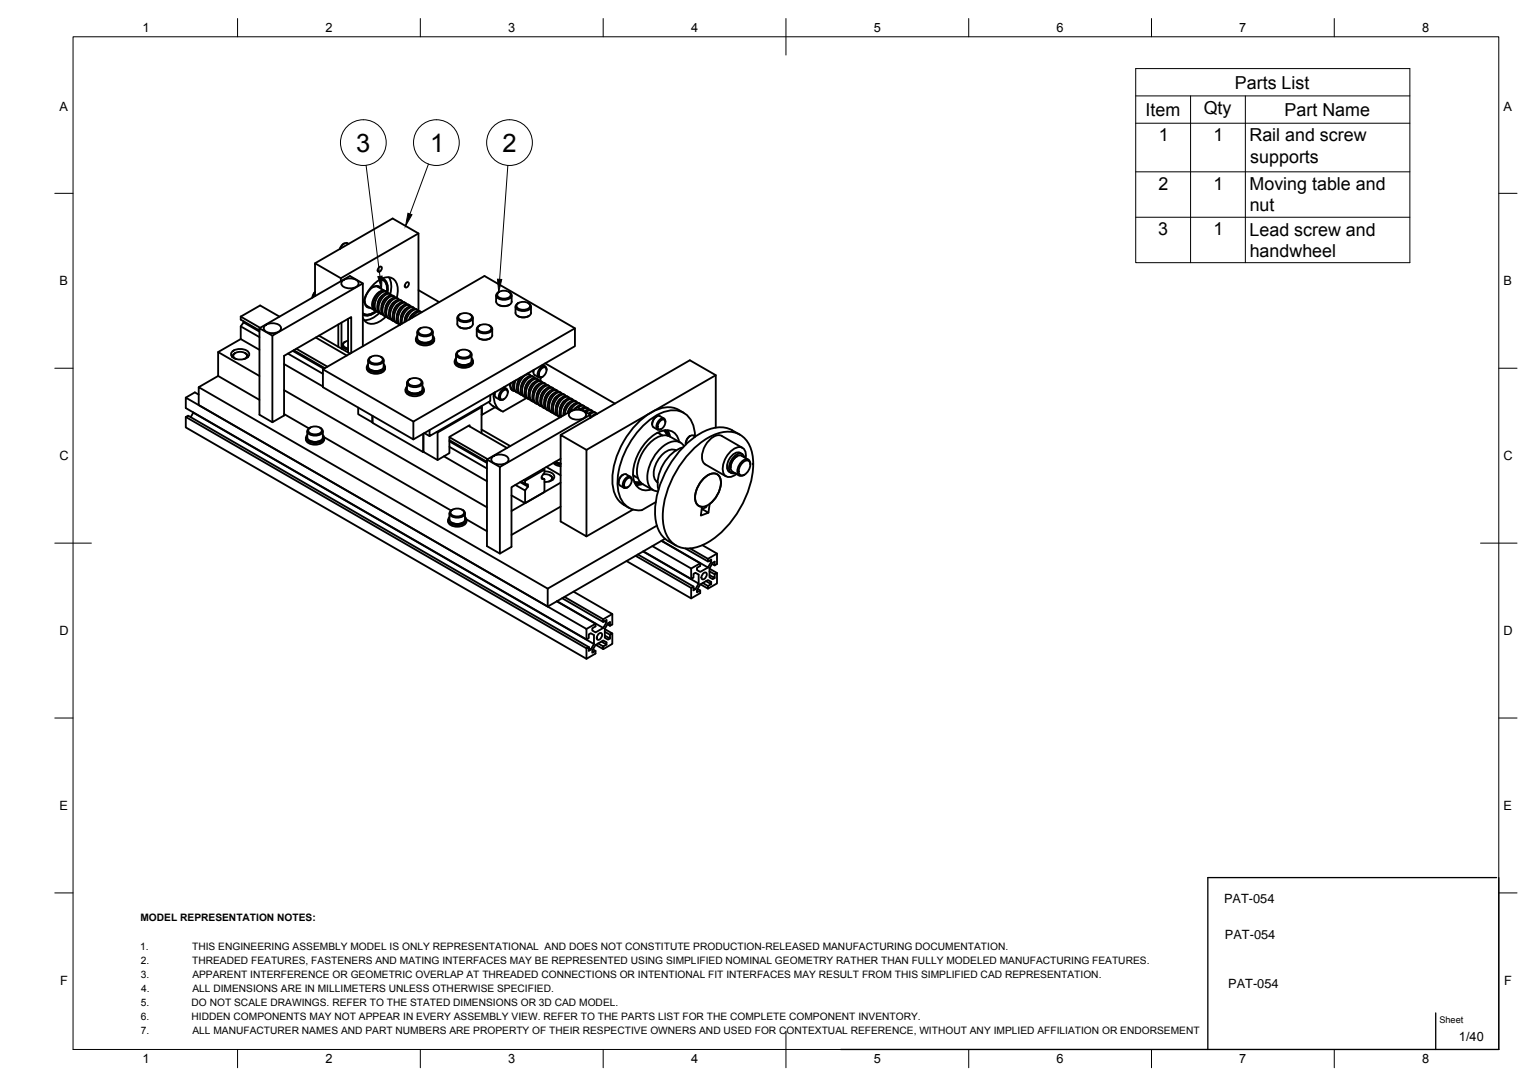
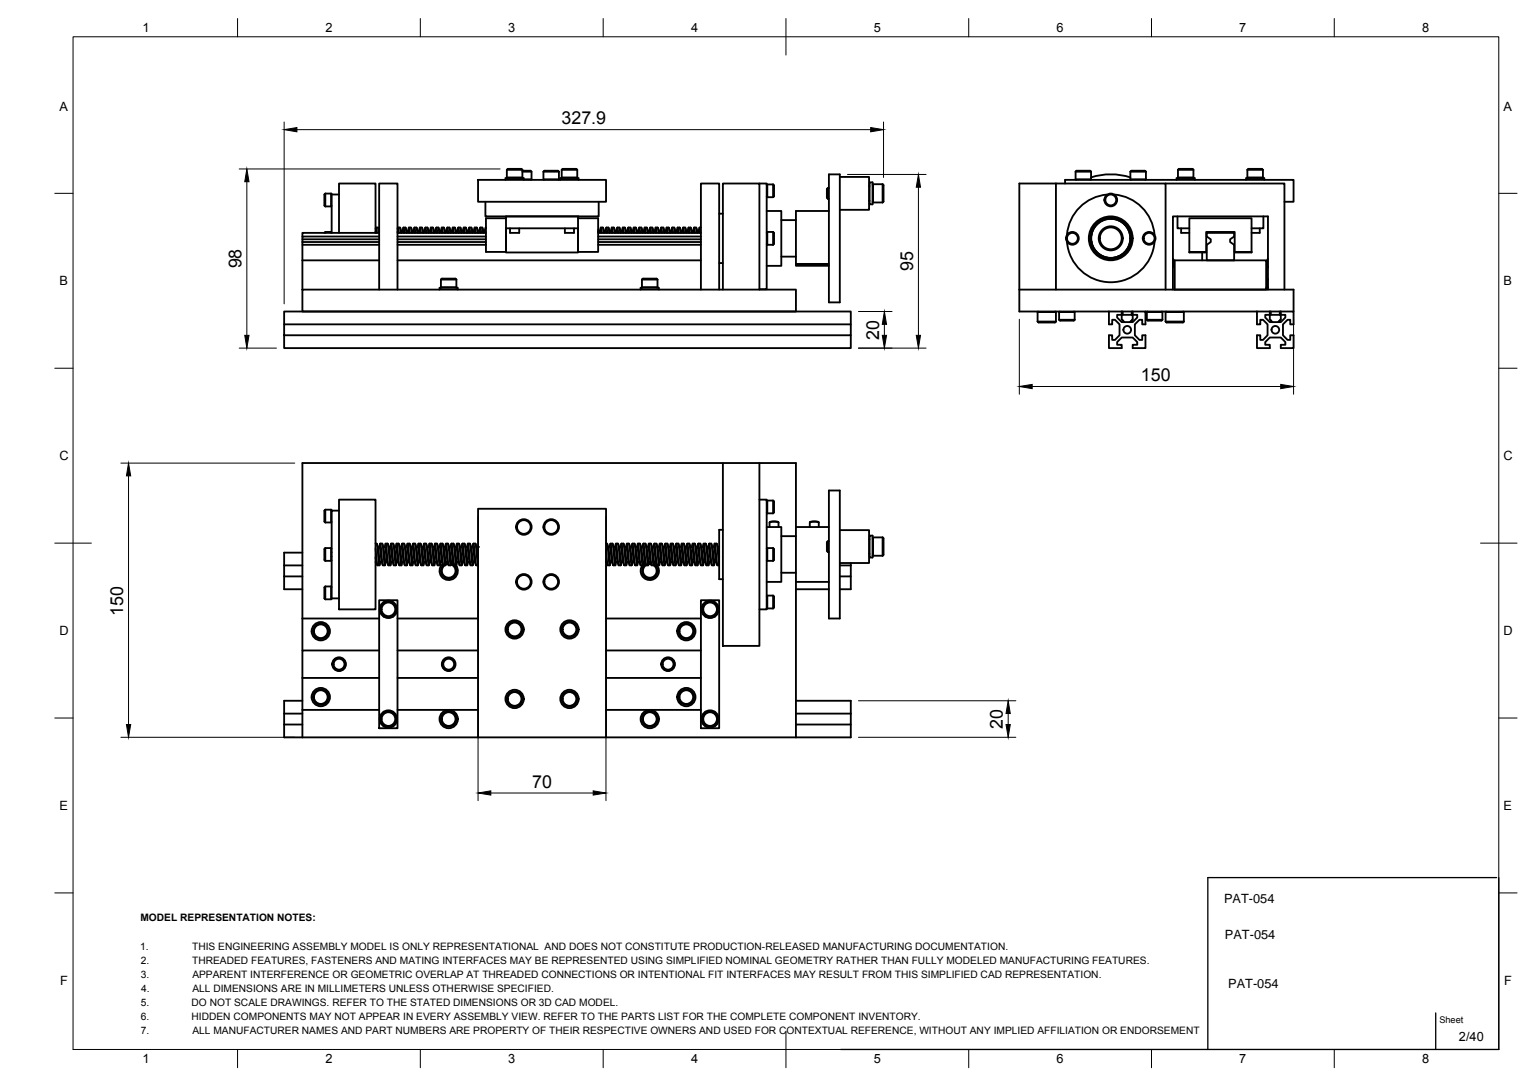
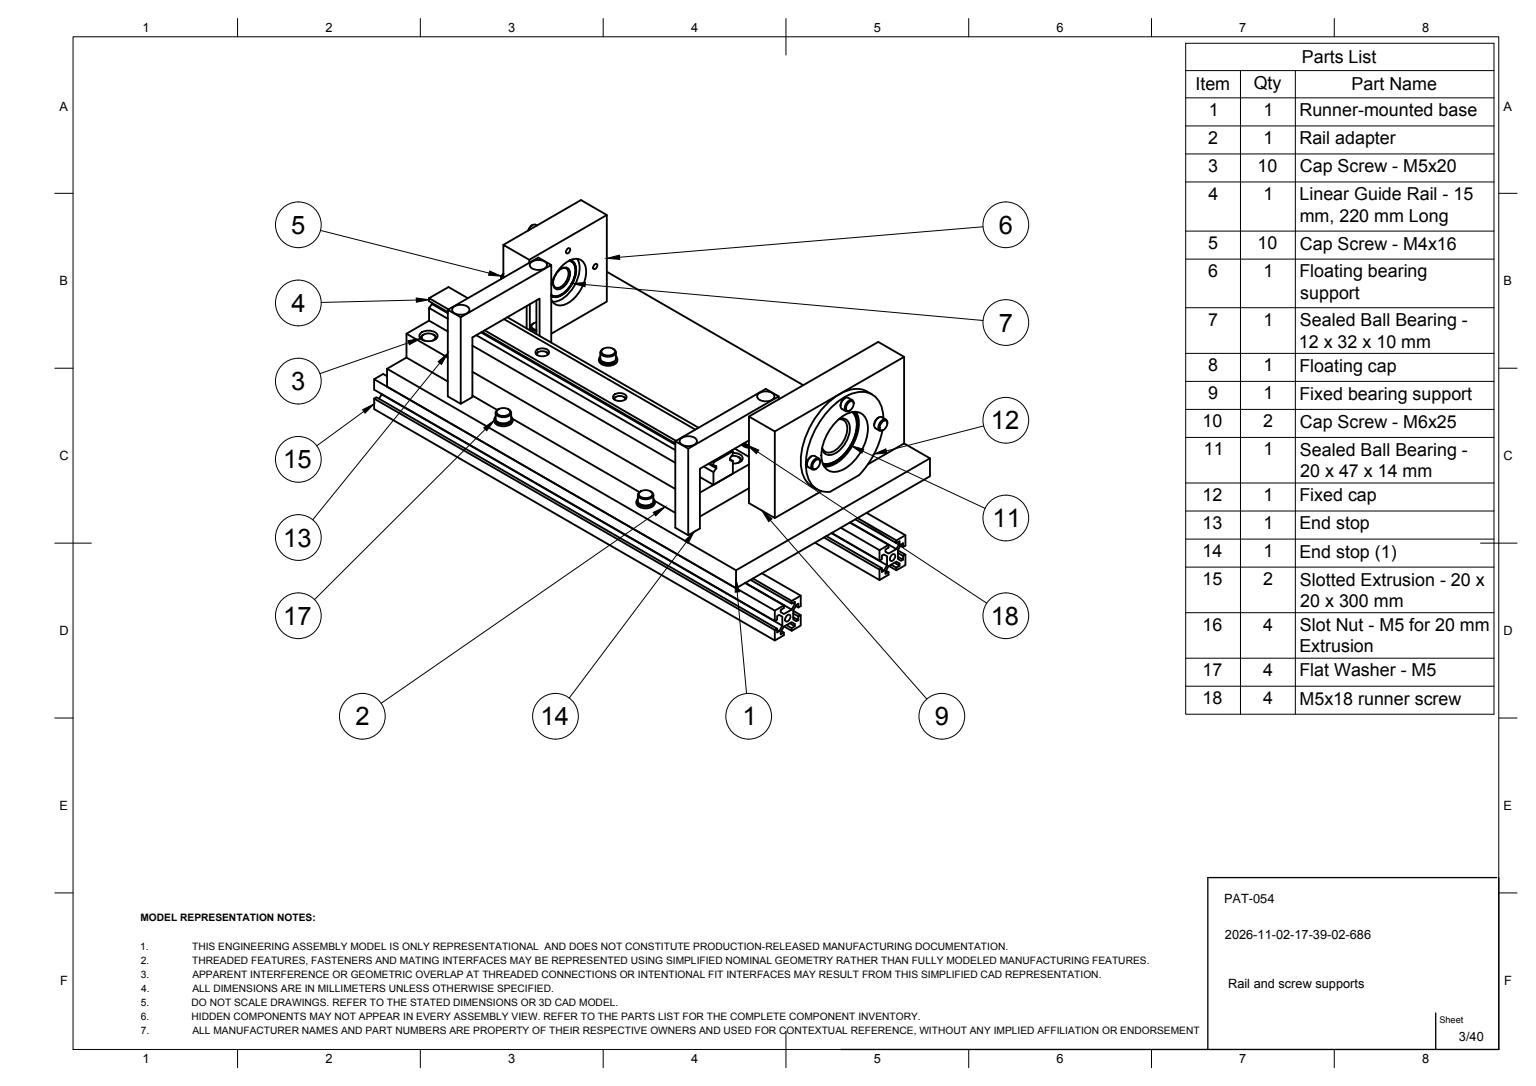
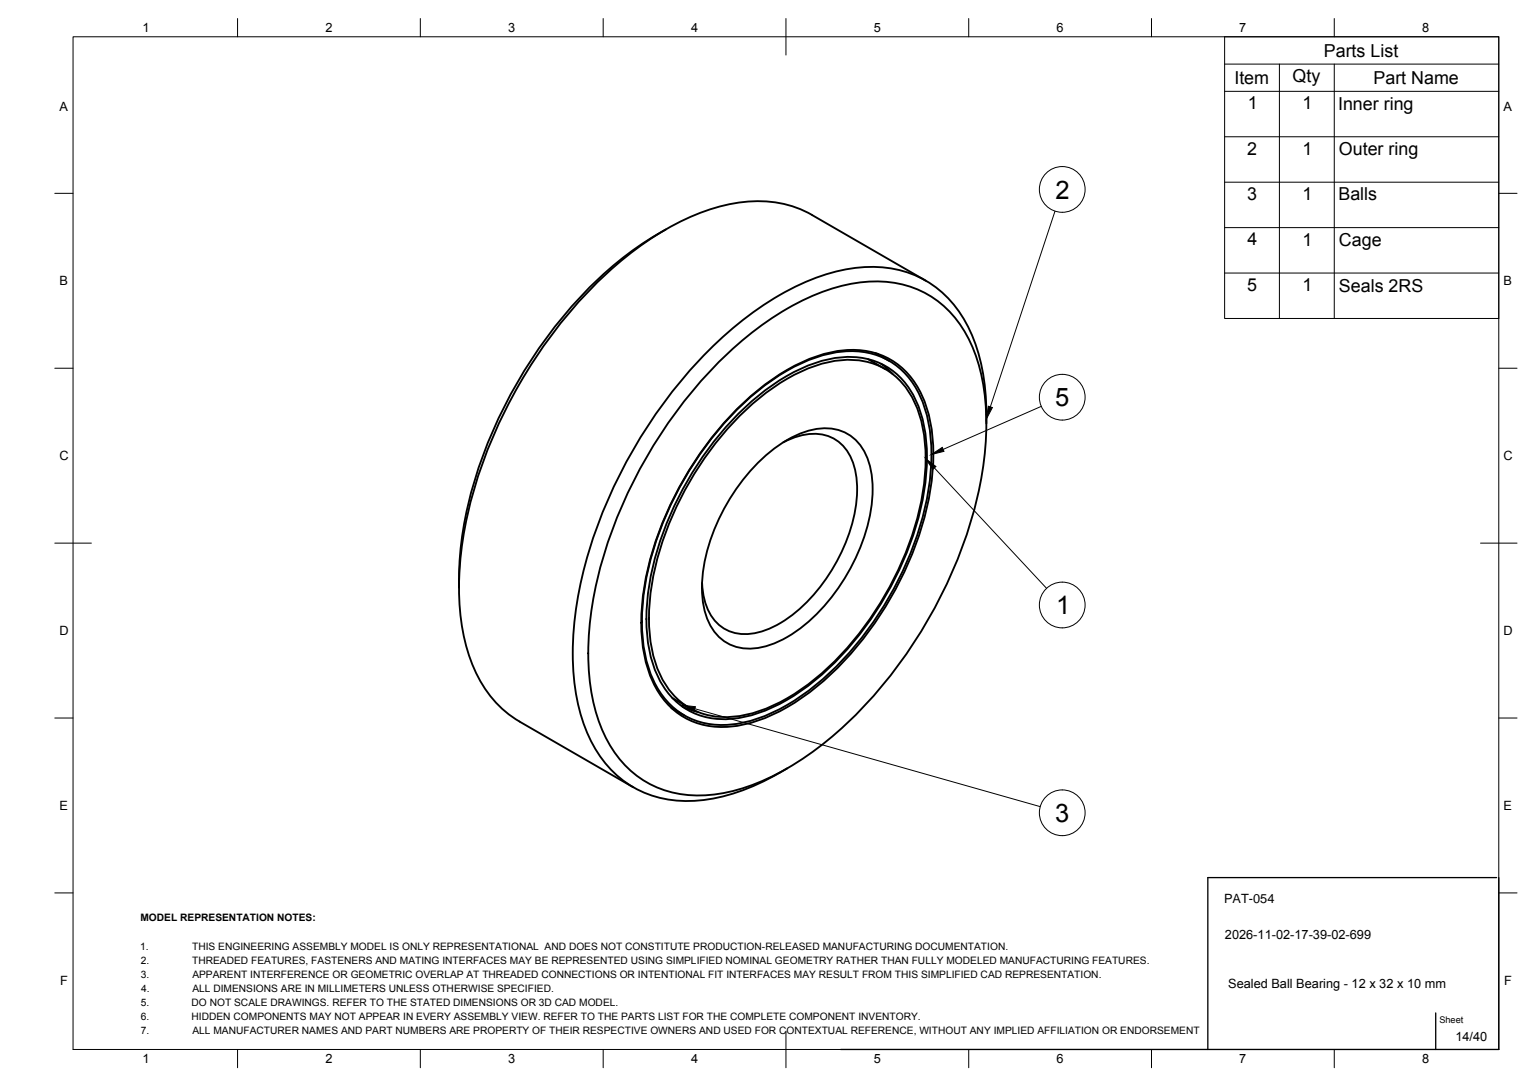
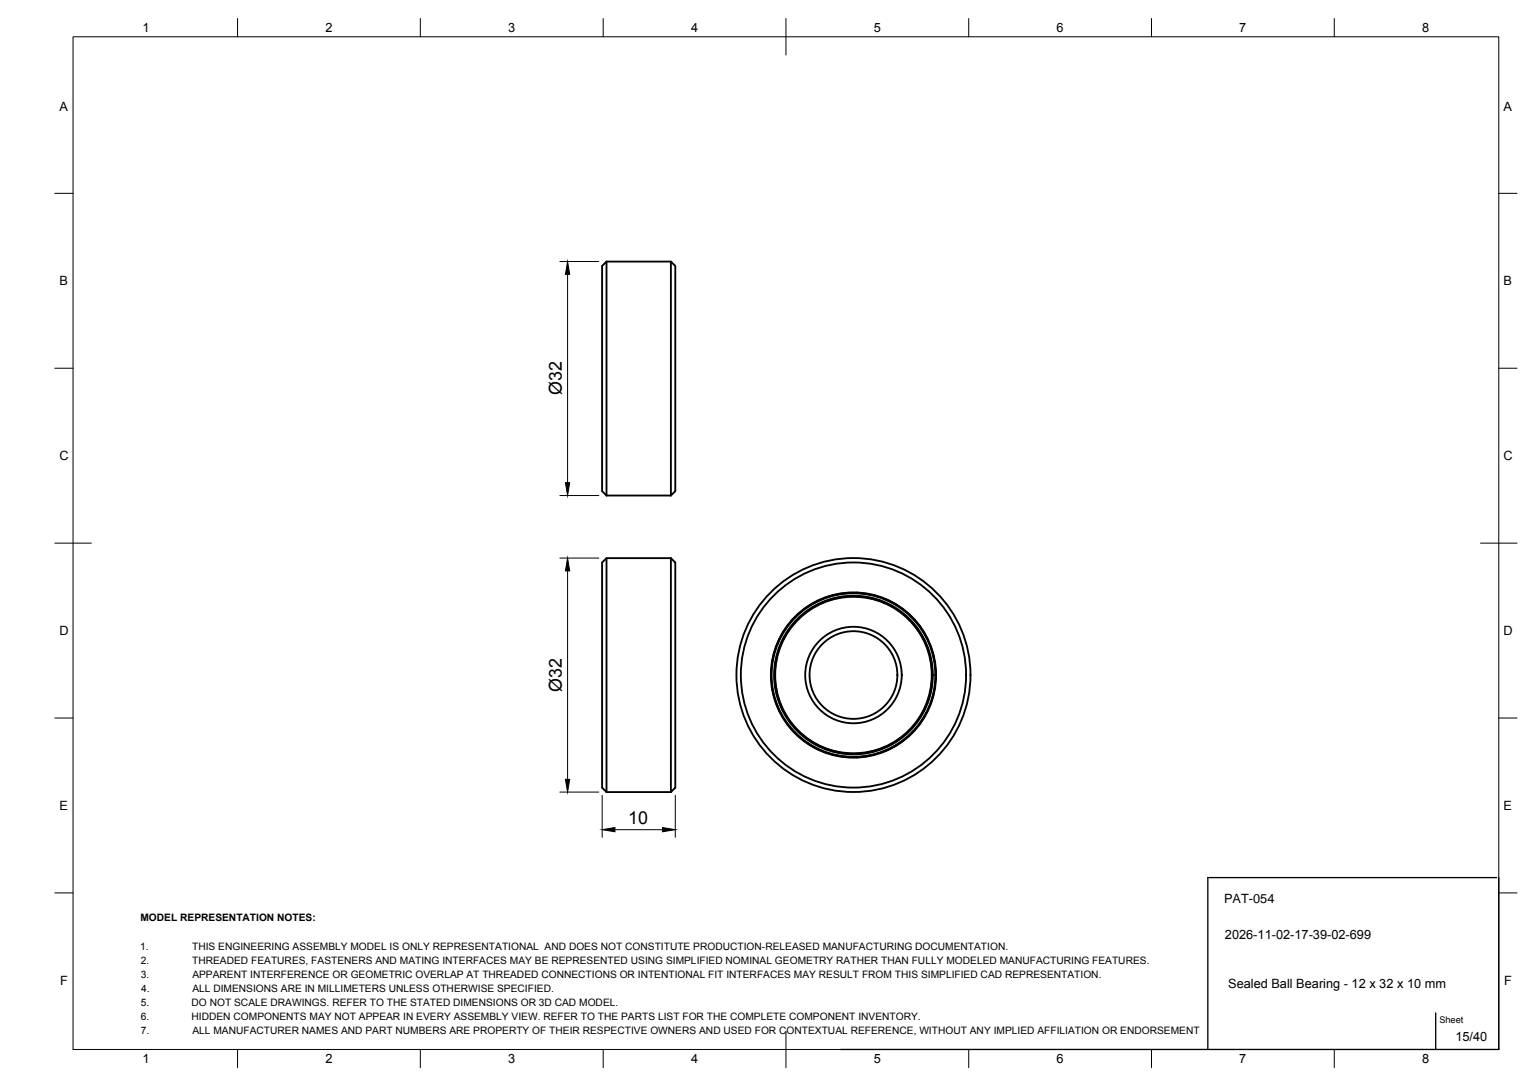
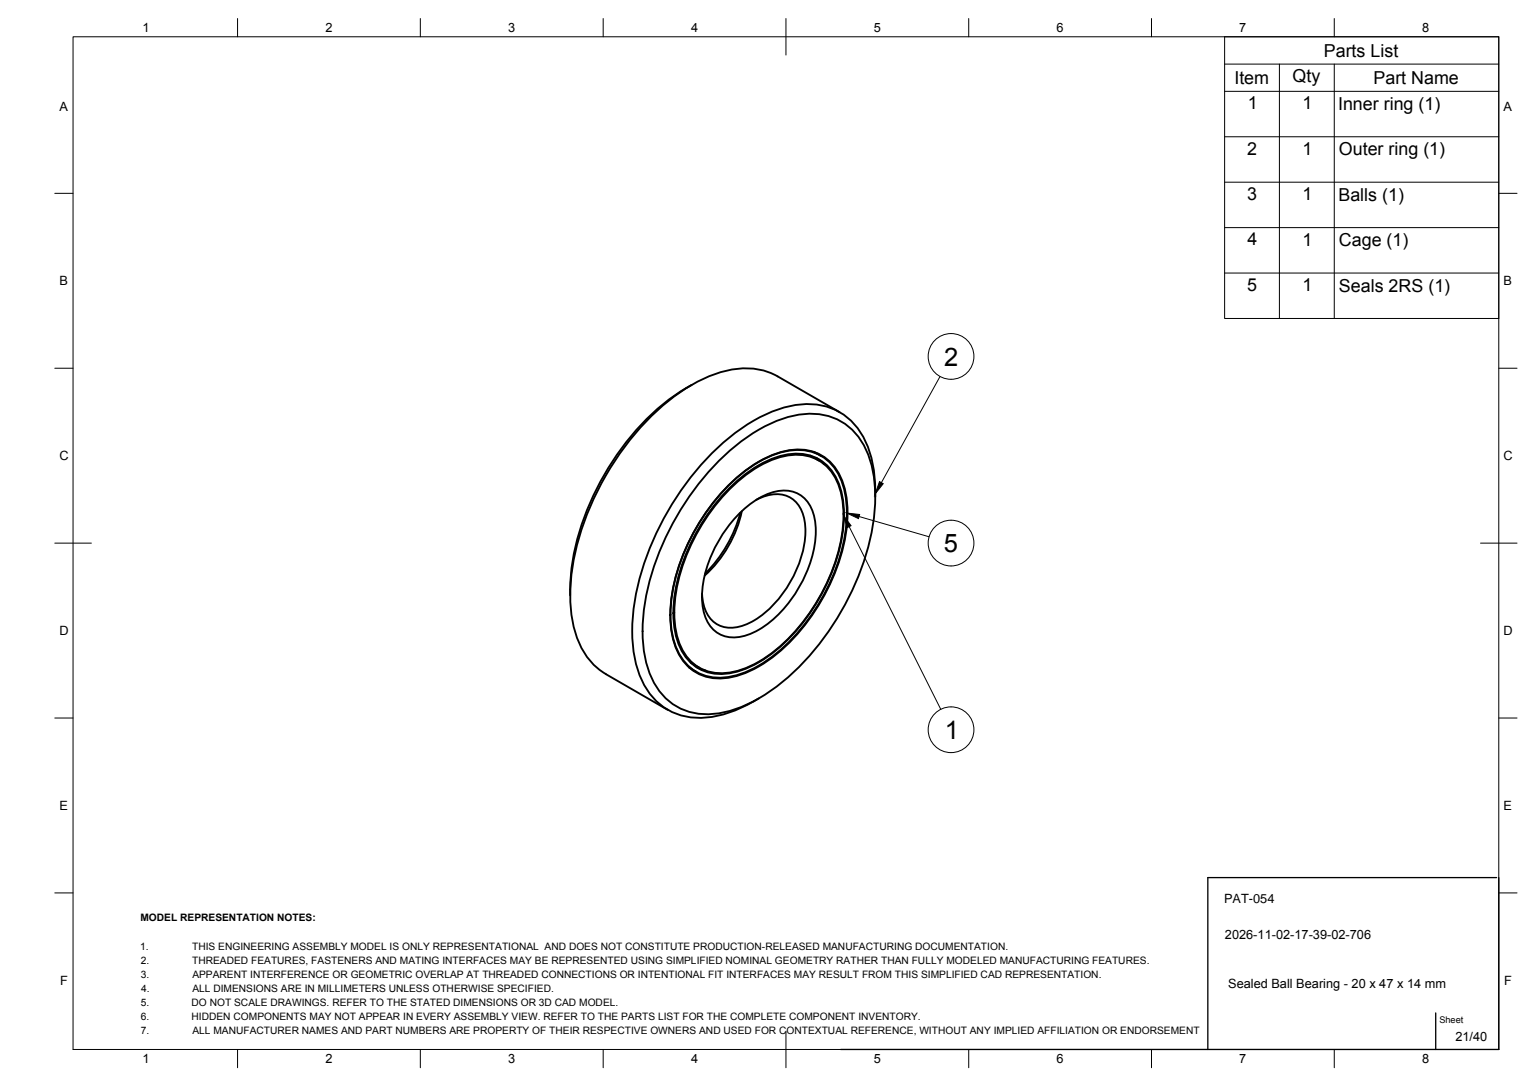
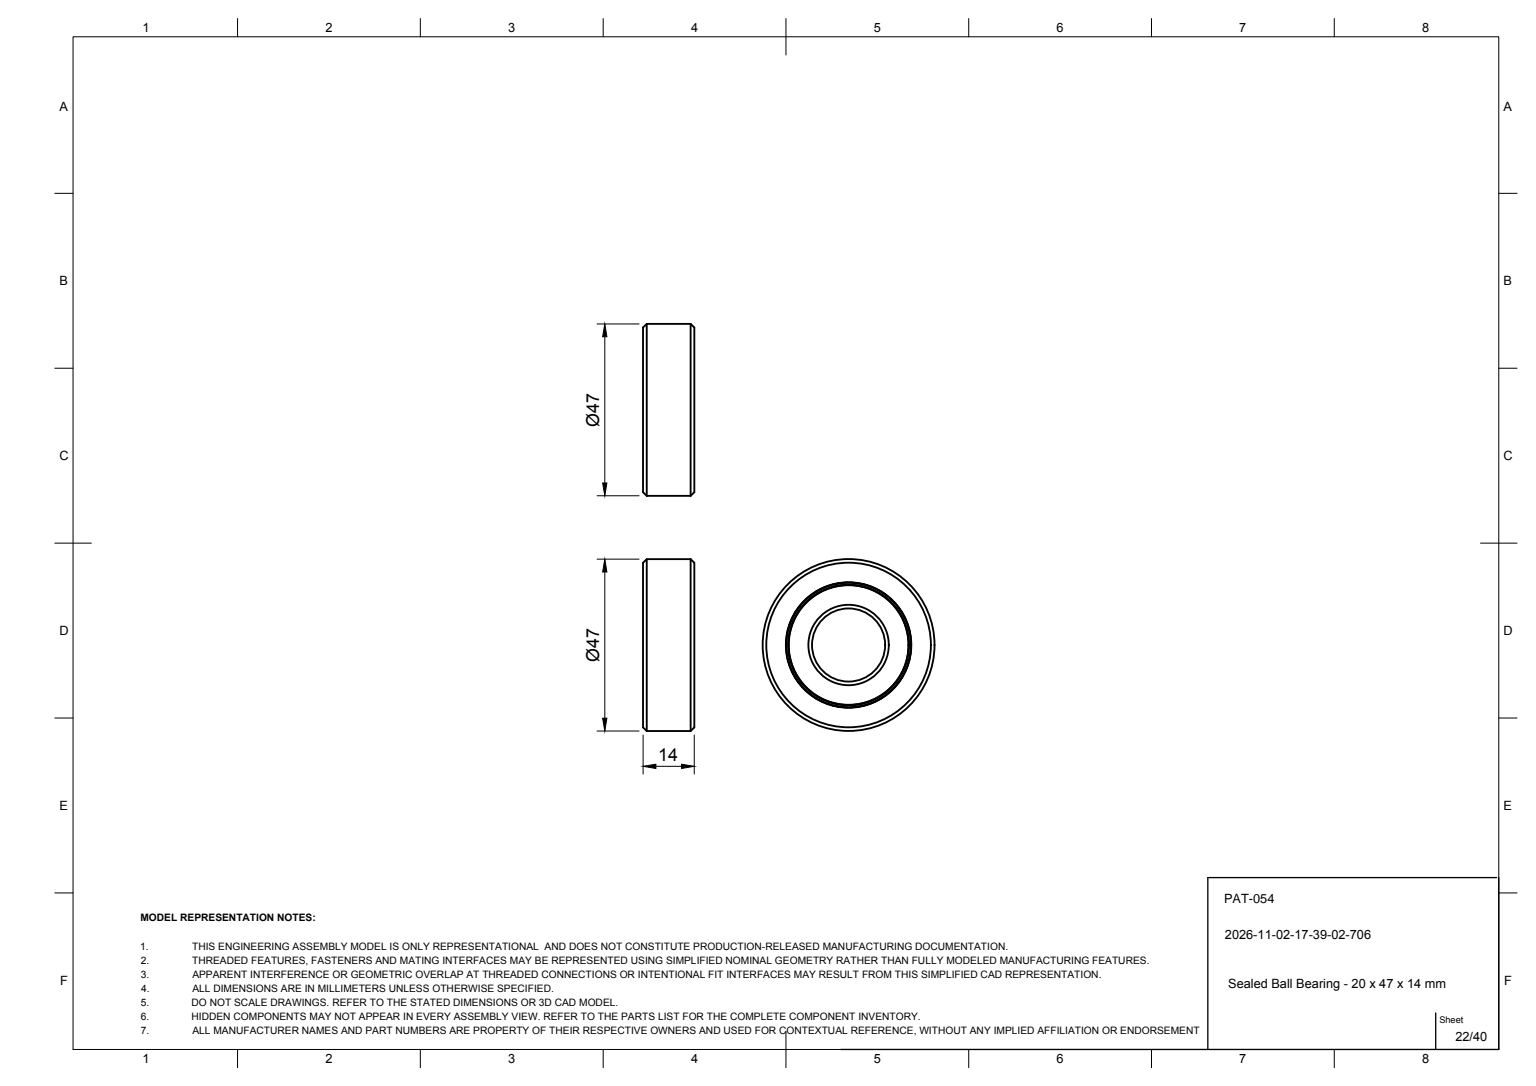
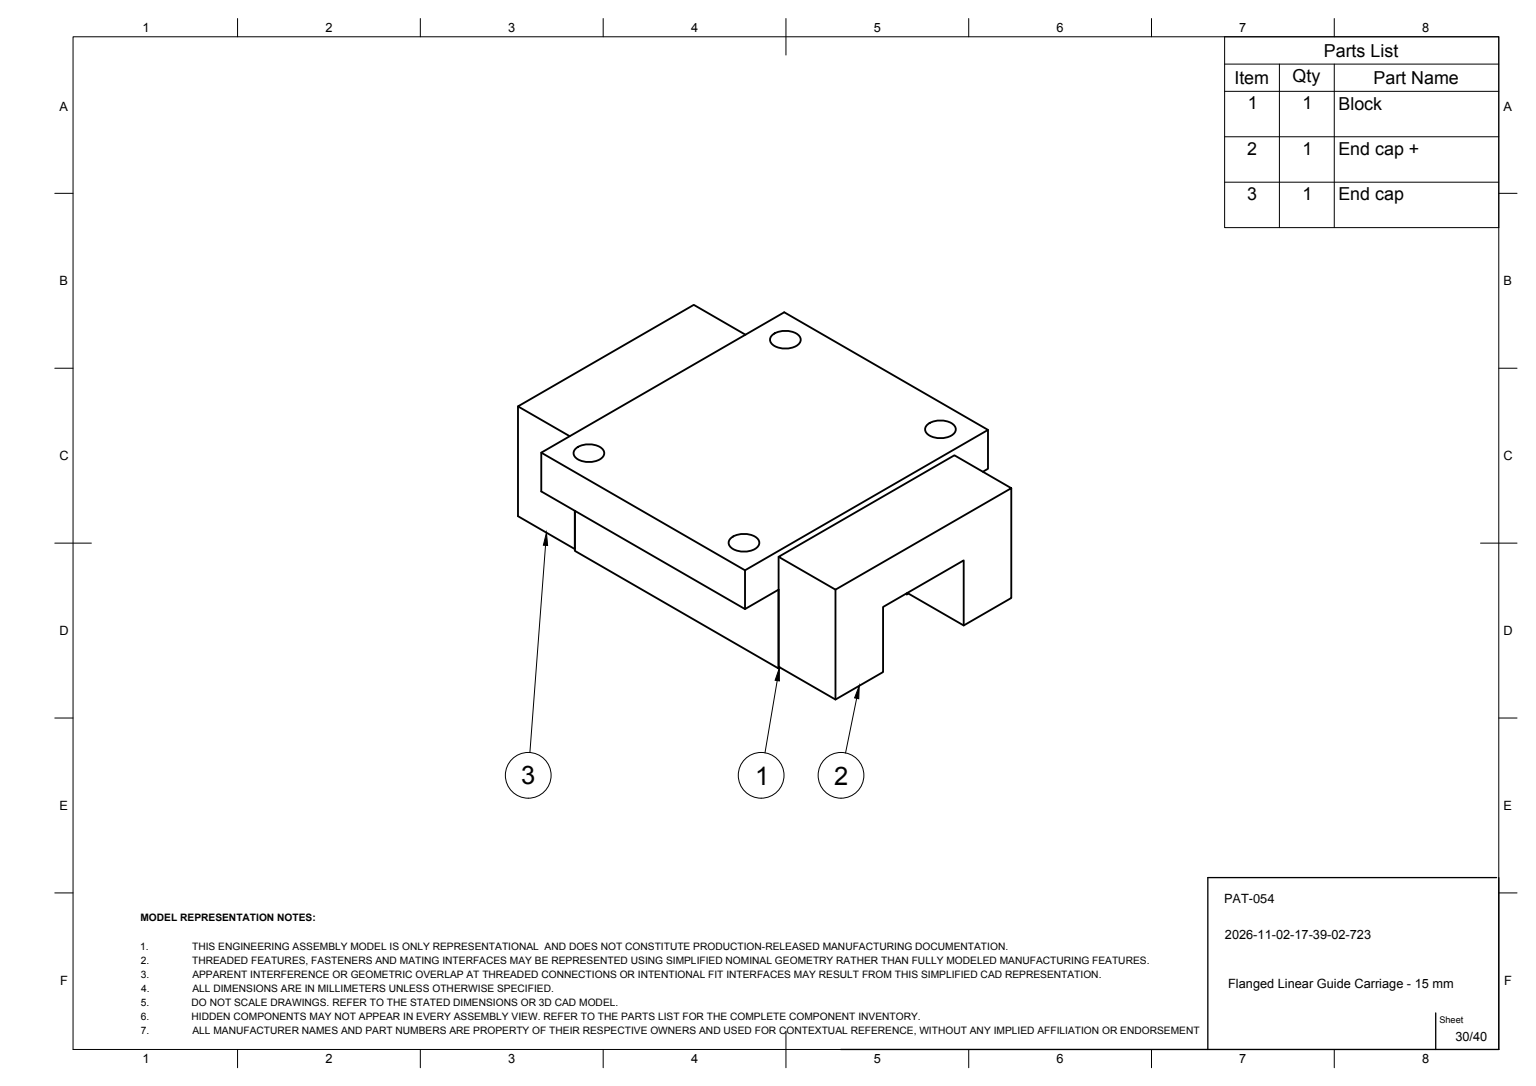
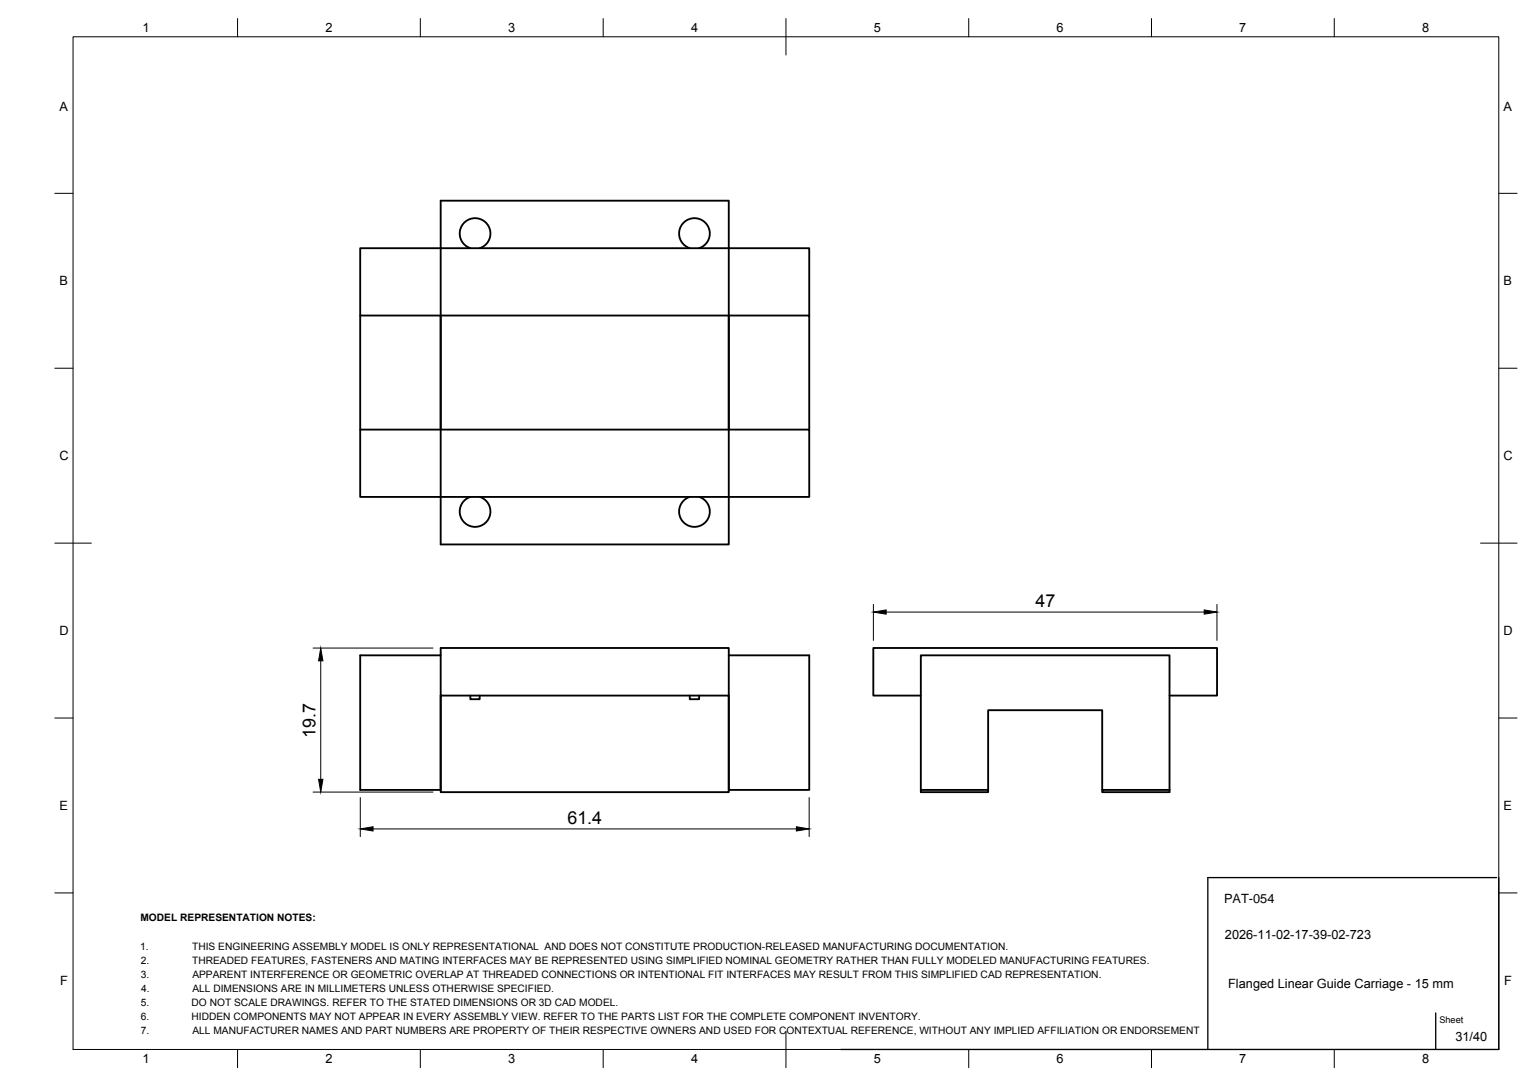
ISO-10303-21;
HEADER;
/* Generated by software containing ST-Developer
 * from STEP Tools, Inc. (www.steptools.com) 
 */

FILE_DESCRIPTION(
/* description */ ('PAT-054'),
/* implementation_level */ '2;1');

FILE_NAME(
/* name */ 'PAT-054',
/* time_stamp */ '2026-10-29T16:38:13-07:00',
/* author */ (''),
/* organization */ (''),
/* preprocessor_version */ 'ST-DEVELOPER v20.2',
/* originating_system */ 'Autodesk Translation Framework v15.17.0.0',
/* authorisation */ '');

FILE_SCHEMA (('AUTOMOTIVE_DESIGN { 1 0 10303 214 3 1 1 }'));
ENDSEC;

DATA;
#10=MECHANICAL_DESIGN_GEOMETRIC_PRESENTATION_REPRESENTATION('',(#899,#900,
#901,#902,#903,#904,#905,#906,#907,#908,#909,#910,#911,#912,#913,#914,#915,
#916,#917,#918,#919,#920,#921,#922,#923,#924,#925,#926,#927,#928,#929,#930,
#931,#932,#933,#934,#935,#936,#937,#938,#939,#940,#941,#942,#943,#944,#945,
#946,#947,#948,#949,#950,#951,#952,#953,#954,#955,#956,#957),#33981);
#11=B_SPLINE_SURFACE_WITH_KNOTS('',3,3,((#22391,#22392,#22393,#22394,#22395,
#22396,#22397,#22398,#22399,#22400,#22401,#22402,#22403,#22404,#22405,#22406,
#22407,#22408,#22409,#22410,#22411,#22412,#22413,#22414,#22415,#22416,#22417,
#22418,#22419,#22420,#22421,#22422,#22423,#22424,#22425,#22426,#22427,#22428,
#22429,#22430,#22431,#22432,#22433,#22434,#22435,#22436,#22437,#22438,#22439,
#22440,#22441,#22442,#22443,#22444,#22445,#22446,#22447,#22448,#22449,#22450,
#22451,#22452,#22453,#22454,#22455,#22456,#22457,#22458,#22459,#22460,#22461,
#22462,#22463,#22464,#22465,#22466,#22467,#22468,#22469,#22470,#22471,#22472,
#22473,#22474,#22475,#22476,#22477,#22478,#22479,#22480,#22481,#22482,#22483,
#22484,#22485,#22486,#22487,#22488,#22489,#22490,#22491,#22492,#22493,#22494,
#22495,#22496,#22497,#22498,#22499,#22500,#22501,#22502,#22503,#22504,#22505),
(#22506,#22507,#22508,#22509,#22510,#22511,#22512,#22513,#22514,#22515,
#22516,#22517,#22518,#22519,#22520,#22521,#22522,#22523,#22524,#22525,#22526,
#22527,#22528,#22529,#22530,#22531,#22532,#22533,#22534,#22535,#22536,#22537,
#22538,#22539,#22540,#22541,#22542,#22543,#22544,#22545,#22546,#22547,#22548,
#22549,#22550,#22551,#22552,#22553,#22554,#22555,#22556,#22557,#22558,#22559,
#22560,#22561,#22562,#22563,#22564,#22565,#22566,#22567,#22568,#22569,#22570,
#22571,#22572,#22573,#22574,#22575,#22576,#22577,#22578,#22579,#22580,#22581,
#22582,#22583,#22584,#22585,#22586,#22587,#22588,#22589,#22590,#22591,#22592,
#22593,#22594,#22595,#22596,#22597,#22598,#22599,#22600,#22601,#22602,#22603,
#22604,#22605,#22606,#22607,#22608,#22609,#22610,#22611,#22612,#22613,#22614,
#22615,#22616,#22617,#22618,#22619,#22620),(#22621,#22622,#22623,#22624,
#22625,#22626,#22627,#22628,#22629,#22630,#22631,#22632,#22633,#22634,#22635,
#22636,#22637,#22638,#22639,#22640,#22641,#22642,#22643,#22644,#22645,#22646,
#22647,#22648,#22649,#22650,#22651,#22652,#22653,#22654,#22655,#22656,#22657,
#22658,#22659,#22660,#22661,#22662,#22663,#22664,#22665,#22666,#22667,#22668,
#22669,#22670,#22671,#22672,#22673,#22674,#22675,#22676,#22677,#22678,#22679,
#22680,#22681,#22682,#22683,#22684,#22685,#22686,#22687,#22688,#22689,#22690,
#22691,#22692,#22693,#22694,#22695,#22696,#22697,#22698,#22699,#22700,#22701,
#22702,#22703,#22704,#22705,#22706,#22707,#22708,#22709,#22710,#22711,#22712,
#22713,#22714,#22715,#22716,#22717,#22718,#22719,#22720,#22721,#22722,#22723,
#22724,#22725,#22726,#22727,#22728,#22729,#22730,#22731,#22732,#22733,#22734,
#22735),(#22736,#22737,#22738,#22739,#22740,#22741,#22742,#22743,#22744,
#22745,#22746,#22747,#22748,#22749,#22750,#22751,#22752,#22753,#22754,#22755,
#22756,#22757,#22758,#22759,#22760,#22761,#22762,#22763,#22764,#22765,#22766,
#22767,#22768,#22769,#22770,#22771,#22772,#22773,#22774,#22775,#22776,#22777,
#22778,#22779,#22780,#22781,#22782,#22783,#22784,#22785,#22786,#22787,#22788,
#22789,#22790,#22791,#22792,#22793,#22794,#22795,#22796,#22797,#22798,#22799,
#22800,#22801,#22802,#22803,#22804,#22805,#22806,#22807,#22808,#22809,#22810,
#22811,#22812,#22813,#22814,#22815,#22816,#22817,#22818,#22819,#22820,#22821,
#22822,#22823,#22824,#22825,#22826,#22827,#22828,#22829,#22830,#22831,#22832,
#22833,#22834,#22835,#22836,#22837,#22838,#22839,#22840,#22841,#22842,#22843,
#22844,#22845,#22846,#22847,#22848,#22849,#22850)),.UNSPECIFIED.,.F.,.F.,
 .F.,(4,4),(4,1,1,1,1,1,1,1,1,1,1,1,1,1,1,1,1,1,1,1,1,1,1,1,1,1,1,1,1,1,
1,1,1,1,1,1,1,1,1,1,1,1,1,1,1,1,1,1,1,1,1,1,1,1,1,1,1,1,1,1,1,1,1,1,1,1,
1,1,1,1,1,1,1,1,1,1,1,1,1,1,1,1,1,1,1,1,1,1,1,1,1,1,1,1,1,1,1,1,1,1,1,1,
1,1,1,1,1,1,1,1,1,1,4),(0.,0.173020531651036),(12.1475814751569,12.6421543672732,
13.1367272593894,13.6313001515056,14.1258730436219,14.6204459357381,15.1150188278544,
15.6095917199706,16.1041646120869,16.5987375042031,17.0933103963194,17.5878832884356,
18.0824561805519,18.5770290726681,19.0716019647843,19.5661748569006,20.0607477490168,
20.5553206411331,21.0498935332493,21.5444664253656,22.0390393174818,22.5336122095981,
23.0281851017143,23.5227579938306,24.0173308859468,24.511903778063,25.0064766701793,
25.5010495622955,25.9956224544118,26.490195346528,26.9847682386443,27.4793411307605,
27.9739140228768,28.468486914993,28.9630598071093,29.4576326992255,29.9522055913417,
30.446778483458,30.9413513755742,31.4359242676905,31.9304971598067,32.425070051923,
32.9196429440392,33.4142158361555,33.9087887282717,34.403361620388,34.8979345125042,
35.3925074046204,35.8870802967367,36.3816531888529,36.8762260809692,37.3707989730854,
37.8653718652017,38.3599447573179,38.8545176494342,39.3490905415504,39.8436634336667,
40.3382363257829,40.8328092178991,41.3273821100154,41.8219550021316,42.3165278942479,
42.8111007863641,43.3056736784804,43.8002465705966,44.2948194627129,44.7893923548291,
45.2839652469454,45.7785381390616,46.2731110311778,46.7676839232941,47.2622568154103,
47.7568297075266,48.2514025996428,48.7459754917591,49.2405483838753,49.7351212759916,
50.2296941681078,50.7242670602241,51.2188399523403,51.7134128444565,52.2079857365728,
52.702558628689,53.1971315208053,53.6917044129215,54.1862773050378,54.680850197154,
55.1754230892703,55.6699959813865,56.1645688735028,56.659141765619,57.1537146577353,
57.6482875498515,58.1428604419677,58.637433334084,59.1320062262002,59.6265791183165,
60.1211520104327,60.615724902549,61.1102977946652,61.6048706867815,62.0994435788977,
62.5940164710139,63.0885893631302,63.5831622552464,64.0777351473627,64.5723080394789,
65.0668809315952,65.5614538237114,66.0560267158277,66.5505996079439,67.0451725000601,
67.5397453921764),.UNSPECIFIED.);
#12=B_SPLINE_SURFACE_WITH_KNOTS('',3,3,((#22950,#22951,#22952,#22953,#22954,
#22955,#22956,#22957,#22958,#22959,#22960,#22961,#22962,#22963,#22964,#22965,
#22966,#22967,#22968,#22969,#22970,#22971,#22972,#22973,#22974,#22975,#22976,
#22977,#22978,#22979,#22980,#22981,#22982,#22983,#22984,#22985,#22986,#22987,
#22988,#22989,#22990,#22991,#22992,#22993,#22994,#22995,#22996,#22997,#22998,
#22999,#23000,#23001,#23002,#23003,#23004,#23005,#23006,#23007,#23008,#23009,
#23010,#23011,#23012,#23013,#23014,#23015,#23016,#23017,#23018,#23019,#23020,
#23021,#23022,#23023,#23024,#23025,#23026,#23027,#23028,#23029,#23030,#23031,
#23032,#23033,#23034,#23035,#23036,#23037,#23038,#23039,#23040,#23041,#23042,
#23043,#23044,#23045,#23046,#23047,#23048,#23049,#23050,#23051,#23052,#23053,
#23054,#23055,#23056,#23057,#23058,#23059,#23060,#23061,#23062,#23063,#23064),
(#23065,#23066,#23067,#23068,#23069,#23070,#23071,#23072,#23073,#23074,
#23075,#23076,#23077,#23078,#23079,#23080,#23081,#23082,#23083,#23084,#23085,
#23086,#23087,#23088,#23089,#23090,#23091,#23092,#23093,#23094,#23095,#23096,
#23097,#23098,#23099,#23100,#23101,#23102,#23103,#23104,#23105,#23106,#23107,
#23108,#23109,#23110,#23111,#23112,#23113,#23114,#23115,#23116,#23117,#23118,
#23119,#23120,#23121,#23122,#23123,#23124,#23125,#23126,#23127,#23128,#23129,
#23130,#23131,#23132,#23133,#23134,#23135,#23136,#23137,#23138,#23139,#23140,
#23141,#23142,#23143,#23144,#23145,#23146,#23147,#23148,#23149,#23150,#23151,
#23152,#23153,#23154,#23155,#23156,#23157,#23158,#23159,#23160,#23161,#23162,
#23163,#23164,#23165,#23166,#23167,#23168,#23169,#23170,#23171,#23172,#23173,
#23174,#23175,#23176,#23177,#23178,#23179),(#23180,#23181,#23182,#23183,
#23184,#23185,#23186,#23187,#23188,#23189,#23190,#23191,#23192,#23193,#23194,
#23195,#23196,#23197,#23198,#23199,#23200,#23201,#23202,#23203,#23204,#23205,
#23206,#23207,#23208,#23209,#23210,#23211,#23212,#23213,#23214,#23215,#23216,
#23217,#23218,#23219,#23220,#23221,#23222,#23223,#23224,#23225,#23226,#23227,
#23228,#23229,#23230,#23231,#23232,#23233,#23234,#23235,#23236,#23237,#23238,
#23239,#23240,#23241,#23242,#23243,#23244,#23245,#23246,#23247,#23248,#23249,
#23250,#23251,#23252,#23253,#23254,#23255,#23256,#23257,#23258,#23259,#23260,
#23261,#23262,#23263,#23264,#23265,#23266,#23267,#23268,#23269,#23270,#23271,
#23272,#23273,#23274,#23275,#23276,#23277,#23278,#23279,#23280,#23281,#23282,
#23283,#23284,#23285,#23286,#23287,#23288,#23289,#23290,#23291,#23292,#23293,
#23294),(#23295,#23296,#23297,#23298,#23299,#23300,#23301,#23302,#23303,
#23304,#23305,#23306,#23307,#23308,#23309,#23310,#23311,#23312,#23313,#23314,
#23315,#23316,#23317,#23318,#23319,#23320,#23321,#23322,#23323,#23324,#23325,
#23326,#23327,#23328,#23329,#23330,#23331,#23332,#23333,#23334,#23335,#23336,
#23337,#23338,#23339,#23340,#23341,#23342,#23343,#23344,#23345,#23346,#23347,
#23348,#23349,#23350,#23351,#23352,#23353,#23354,#23355,#23356,#23357,#23358,
#23359,#23360,#23361,#23362,#23363,#23364,#23365,#23366,#23367,#23368,#23369,
#23370,#23371,#23372,#23373,#23374,#23375,#23376,#23377,#23378,#23379,#23380,
#23381,#23382,#23383,#23384,#23385,#23386,#23387,#23388,#23389,#23390,#23391,
#23392,#23393,#23394,#23395,#23396,#23397,#23398,#23399,#23400,#23401,#23402,
#23403,#23404,#23405,#23406,#23407,#23408,#23409)),.UNSPECIFIED.,.F.,.F.,
 .F.,(4,4),(4,1,1,1,1,1,1,1,1,1,1,1,1,1,1,1,1,1,1,1,1,1,1,1,1,1,1,1,1,1,
1,1,1,1,1,1,1,1,1,1,1,1,1,1,1,1,1,1,1,1,1,1,1,1,1,1,1,1,1,1,1,1,1,1,1,1,
1,1,1,1,1,1,1,1,1,1,1,1,1,1,1,1,1,1,1,1,1,1,1,1,1,1,1,1,1,1,1,1,1,1,1,1,
1,1,1,1,1,1,1,1,1,1,4),(0.,0.173020531651036),(15.1888611523549,15.6834340444711,
16.1780069365874,16.6725798287036,17.1671527208199,17.6617256129361,18.1562985050523,
18.6508713971686,19.1454442892848,19.6400171814011,20.1345900735173,20.6291629656336,
21.1237358577498,21.6183087498661,22.1128816419823,22.6074545340986,23.1020274262148,
23.596600318331,24.0911732104473,24.5857461025635,25.0803189946798,25.574891886796,
26.0694647789123,26.5640376710285,27.0586105631448,27.553183455261,28.0477563473773,
28.5423292394935,29.0369021316097,29.531475023726,30.0260479158422,30.5206208079585,
31.0151937000747,31.509766592191,32.0043394843072,32.4989123764235,32.9934852685397,
33.488058160656,33.9826310527722,34.4772039448884,34.9717768370047,35.4663497291209,
35.9609226212372,36.4554955133534,36.9500684054697,37.4446412975859,37.9392141897022,
38.4337870818184,38.9283599739347,39.4229328660509,39.9175057581671,40.4120786502834,
40.9066515423996,41.4012244345159,41.8957973266321,42.3903702187484,42.8849431108646,
43.3795160029809,43.8740888950971,44.3686617872134,44.8632346793296,45.3578075714458,
45.8523804635621,46.3469533556783,46.8415262477946,47.3360991399108,47.8306720320271,
48.3252449241433,48.8198178162596,49.3143907083758,49.8089636004921,50.3035364926083,
50.7981093847245,51.2926822768408,51.787255168957,52.2818280610733,52.7764009531895,
53.2709738453058,53.765546737422,54.2601196295383,54.7546925216545,55.2492654137708,
55.743838305887,56.2384111980032,56.7329840901195,57.2275569822357,57.722129874352,
58.2167027664682,58.7112756585845,59.2058485507007,59.700421442817,60.1949943349332,
60.6895672270495,61.1841401191657,61.6787130112819,62.1732859033982,62.6678587955144,
63.1624316876307,63.6570045797469,64.1515774718632,64.6461503639794,65.1407232560957,
65.6352961482119,66.1298690403281,66.6244419324444,67.1190148245607,67.6135877166769,
68.1081606087931,68.6027335009094,69.0973063930256,69.5918792851419,70.0864521772581,
70.5810250693744),.UNSPECIFIED.);
#13=B_SPLINE_SURFACE_WITH_KNOTS('',3,3,((#29192,#29193,#29194,#29195,#29196,
#29197,#29198,#29199,#29200,#29201,#29202,#29203,#29204,#29205,#29206,#29207,
#29208,#29209,#29210,#29211,#29212,#29213,#29214,#29215,#29216,#29217,#29218,
#29219,#29220,#29221,#29222,#29223,#29224,#29225,#29226,#29227,#29228,#29229,
#29230,#29231,#29232,#29233,#29234,#29235,#29236,#29237,#29238,#29239,#29240,
#29241,#29242,#29243,#29244,#29245,#29246,#29247,#29248,#29249,#29250,#29251,
#29252,#29253,#29254,#29255,#29256,#29257,#29258,#29259,#29260,#29261,#29262,
#29263,#29264,#29265,#29266,#29267,#29268,#29269,#29270,#29271,#29272,#29273,
#29274,#29275,#29276,#29277,#29278,#29279,#29280,#29281,#29282,#29283,#29284,
#29285,#29286,#29287,#29288,#29289,#29290,#29291,#29292,#29293,#29294,#29295,
#29296,#29297,#29298,#29299,#29300,#29301,#29302,#29303,#29304,#29305,#29306,
#29307,#29308,#29309,#29310,#29311,#29312,#29313,#29314,#29315,#29316,#29317,
#29318,#29319,#29320,#29321,#29322,#29323,#29324,#29325,#29326,#29327,#29328,
#29329,#29330,#29331,#29332,#29333,#29334,#29335,#29336,#29337,#29338,#29339,
#29340,#29341,#29342,#29343,#29344,#29345,#29346,#29347,#29348,#29349,#29350,
#29351,#29352,#29353,#29354,#29355,#29356,#29357,#29358,#29359,#29360,#29361,
#29362,#29363,#29364,#29365,#29366,#29367,#29368,#29369,#29370,#29371,#29372,
#29373,#29374,#29375,#29376,#29377,#29378,#29379,#29380,#29381,#29382,#29383,
#29384,#29385,#29386,#29387,#29388,#29389,#29390,#29391,#29392,#29393,#29394,
#29395,#29396,#29397,#29398,#29399,#29400,#29401,#29402,#29403,#29404,#29405,
#29406,#29407,#29408,#29409,#29410,#29411,#29412,#29413,#29414,#29415,#29416,
#29417,#29418,#29419,#29420,#29421,#29422,#29423,#29424,#29425,#29426,#29427,
#29428,#29429,#29430,#29431,#29432,#29433,#29434,#29435,#29436,#29437,#29438,
#29439,#29440,#29441,#29442,#29443,#29444,#29445,#29446,#29447,#29448,#29449,
#29450,#29451,#29452,#29453,#29454,#29455,#29456,#29457,#29458,#29459,#29460,
#29461,#29462,#29463,#29464,#29465,#29466,#29467,#29468,#29469,#29470,#29471,
#29472,#29473,#29474,#29475,#29476,#29477,#29478,#29479,#29480,#29481,#29482,
#29483,#29484,#29485,#29486,#29487,#29488,#29489,#29490,#29491,#29492,#29493,
#29494,#29495,#29496,#29497,#29498,#29499,#29500,#29501,#29502,#29503,#29504,
#29505,#29506,#29507,#29508,#29509,#29510,#29511,#29512,#29513,#29514,#29515,
#29516,#29517,#29518,#29519,#29520,#29521,#29522,#29523,#29524,#29525,#29526,
#29527,#29528,#29529,#29530,#29531,#29532,#29533,#29534,#29535,#29536,#29537,
#29538,#29539,#29540,#29541,#29542,#29543,#29544,#29545,#29546,#29547,#29548,
#29549,#29550,#29551,#29552,#29553,#29554,#29555,#29556,#29557,#29558,#29559,
#29560,#29561,#29562,#29563,#29564,#29565,#29566,#29567,#29568,#29569,#29570,
#29571,#29572,#29573,#29574,#29575,#29576,#29577,#29578,#29579,#29580,#29581,
#29582,#29583,#29584,#29585,#29586,#29587,#29588,#29589,#29590,#29591,#29592,
#29593,#29594,#29595,#29596,#29597,#29598,#29599,#29600,#29601,#29602,#29603,
#29604,#29605,#29606,#29607,#29608,#29609,#29610,#29611,#29612,#29613,#29614,
#29615,#29616,#29617,#29618,#29619,#29620,#29621,#29622,#29623,#29624,#29625,
#29626,#29627,#29628,#29629,#29630,#29631,#29632,#29633,#29634,#29635,#29636,
#29637,#29638,#29639,#29640,#29641,#29642,#29643,#29644,#29645,#29646,#29647,
#29648,#29649,#29650,#29651,#29652,#29653,#29654,#29655,#29656,#29657,#29658,
#29659,#29660,#29661,#29662,#29663,#29664,#29665,#29666,#29667,#29668,#29669,
#29670,#29671,#29672,#29673,#29674,#29675,#29676,#29677,#29678,#29679,#29680,
#29681,#29682,#29683,#29684,#29685,#29686,#29687,#29688,#29689),(#29690,
#29691,#29692,#29693,#29694,#29695,#29696,#29697,#29698,#29699,#29700,#29701,
#29702,#29703,#29704,#29705,#29706,#29707,#29708,#29709,#29710,#29711,#29712,
#29713,#29714,#29715,#29716,#29717,#29718,#29719,#29720,#29721,#29722,#29723,
#29724,#29725,#29726,#29727,#29728,#29729,#29730,#29731,#29732,#29733,#29734,
#29735,#29736,#29737,#29738,#29739,#29740,#29741,#29742,#29743,#29744,#29745,
#29746,#29747,#29748,#29749,#29750,#29751,#29752,#29753,#29754,#29755,#29756,
#29757,#29758,#29759,#29760,#29761,#29762,#29763,#29764,#29765,#29766,#29767,
#29768,#29769,#29770,#29771,#29772,#29773,#29774,#29775,#29776,#29777,#29778,
#29779,#29780,#29781,#29782,#29783,#29784,#29785,#29786,#29787,#29788,#29789,
#29790,#29791,#29792,#29793,#29794,#29795,#29796,#29797,#29798,#29799,#29800,
#29801,#29802,#29803,#29804,#29805,#29806,#29807,#29808,#29809,#29810,#29811,
#29812,#29813,#29814,#29815,#29816,#29817,#29818,#29819,#29820,#29821,#29822,
#29823,#29824,#29825,#29826,#29827,#29828,#29829,#29830,#29831,#29832,#29833,
#29834,#29835,#29836,#29837,#29838,#29839,#29840,#29841,#29842,#29843,#29844,
#29845,#29846,#29847,#29848,#29849,#29850,#29851,#29852,#29853,#29854,#29855,
#29856,#29857,#29858,#29859,#29860,#29861,#29862,#29863,#29864,#29865,#29866,
#29867,#29868,#29869,#29870,#29871,#29872,#29873,#29874,#29875,#29876,#29877,
#29878,#29879,#29880,#29881,#29882,#29883,#29884,#29885,#29886,#29887,#29888,
#29889,#29890,#29891,#29892,#29893,#29894,#29895,#29896,#29897,#29898,#29899,
#29900,#29901,#29902,#29903,#29904,#29905,#29906,#29907,#29908,#29909,#29910,
#29911,#29912,#29913,#29914,#29915,#29916,#29917,#29918,#29919,#29920,#29921,
#29922,#29923,#29924,#29925,#29926,#29927,#29928,#29929,#29930,#29931,#29932,
#29933,#29934,#29935,#29936,#29937,#29938,#29939,#29940,#29941,#29942,#29943,
#29944,#29945,#29946,#29947,#29948,#29949,#29950,#29951,#29952,#29953,#29954,
#29955,#29956,#29957,#29958,#29959,#29960,#29961,#29962,#29963,#29964,#29965,
#29966,#29967,#29968,#29969,#29970,#29971,#29972,#29973,#29974,#29975,#29976,
#29977,#29978,#29979,#29980,#29981,#29982,#29983,#29984,#29985,#29986,#29987,
#29988,#29989,#29990,#29991,#29992,#29993,#29994,#29995,#29996,#29997,#29998,
#29999,#30000,#30001,#30002,#30003,#30004,#30005,#30006,#30007,#30008,#30009,
#30010,#30011,#30012,#30013,#30014,#30015,#30016,#30017,#30018,#30019,#30020,
#30021,#30022,#30023,#30024,#30025,#30026,#30027,#30028,#30029,#30030,#30031,
#30032,#30033,#30034,#30035,#30036,#30037,#30038,#30039,#30040,#30041,#30042,
#30043,#30044,#30045,#30046,#30047,#30048,#30049,#30050,#30051,#30052,#30053,
#30054,#30055,#30056,#30057,#30058,#30059,#30060,#30061,#30062,#30063,#30064,
#30065,#30066,#30067,#30068,#30069,#30070,#30071,#30072,#30073,#30074,#30075,
#30076,#30077,#30078,#30079,#30080,#30081,#30082,#30083,#30084,#30085,#30086,
#30087,#30088,#30089,#30090,#30091,#30092,#30093,#30094,#30095,#30096,#30097,
#30098,#30099,#30100,#30101,#30102,#30103,#30104,#30105,#30106,#30107,#30108,
#30109,#30110,#30111,#30112,#30113,#30114,#30115,#30116,#30117,#30118,#30119,
#30120,#30121,#30122,#30123,#30124,#30125,#30126,#30127,#30128,#30129,#30130,
#30131,#30132,#30133,#30134,#30135,#30136,#30137,#30138,#30139,#30140,#30141,
#30142,#30143,#30144,#30145,#30146,#30147,#30148,#30149,#30150,#30151,#30152,
#30153,#30154,#30155,#30156,#30157,#30158,#30159,#30160,#30161,#30162,#30163,
#30164,#30165,#30166,#30167,#30168,#30169,#30170,#30171,#30172,#30173,#30174,
#30175,#30176,#30177,#30178,#30179,#30180,#30181,#30182,#30183,#30184,#30185,
#30186,#30187),(#30188,#30189,#30190,#30191,#30192,#30193,#30194,#30195,
#30196,#30197,#30198,#30199,#30200,#30201,#30202,#30203,#30204,#30205,#30206,
#30207,#30208,#30209,#30210,#30211,#30212,#30213,#30214,#30215,#30216,#30217,
#30218,#30219,#30220,#30221,#30222,#30223,#30224,#30225,#30226,#30227,#30228,
#30229,#30230,#30231,#30232,#30233,#30234,#30235,#30236,#30237,#30238,#30239,
#30240,#30241,#30242,#30243,#30244,#30245,#30246,#30247,#30248,#30249,#30250,
#30251,#30252,#30253,#30254,#30255,#30256,#30257,#30258,#30259,#30260,#30261,
#30262,#30263,#30264,#30265,#30266,#30267,#30268,#30269,#30270,#30271,#30272,
#30273,#30274,#30275,#30276,#30277,#30278,#30279,#30280,#30281,#30282,#30283,
#30284,#30285,#30286,#30287,#30288,#30289,#30290,#30291,#30292,#30293,#30294,
#30295,#30296,#30297,#30298,#30299,#30300,#30301,#30302,#30303,#30304,#30305,
#30306,#30307,#30308,#30309,#30310,#30311,#30312,#30313,#30314,#30315,#30316,
#30317,#30318,#30319,#30320,#30321,#30322,#30323,#30324,#30325,#30326,#30327,
#30328,#30329,#30330,#30331,#30332,#30333,#30334,#30335,#30336,#30337,#30338,
#30339,#30340,#30341,#30342,#30343,#30344,#30345,#30346,#30347,#30348,#30349,
#30350,#30351,#30352,#30353,#30354,#30355,#30356,#30357,#30358,#30359,#30360,
#30361,#30362,#30363,#30364,#30365,#30366,#30367,#30368,#30369,#30370,#30371,
#30372,#30373,#30374,#30375,#30376,#30377,#30378,#30379,#30380,#30381,#30382,
#30383,#30384,#30385,#30386,#30387,#30388,#30389,#30390,#30391,#30392,#30393,
#30394,#30395,#30396,#30397,#30398,#30399,#30400,#30401,#30402,#30403,#30404,
#30405,#30406,#30407,#30408,#30409,#30410,#30411,#30412,#30413,#30414,#30415,
#30416,#30417,#30418,#30419,#30420,#30421,#30422,#30423,#30424,#30425,#30426,
#30427,#30428,#30429,#30430,#30431,#30432,#30433,#30434,#30435,#30436,#30437,
#30438,#30439,#30440,#30441,#30442,#30443,#30444,#30445,#30446,#30447,#30448,
#30449,#30450,#30451,#30452,#30453,#30454,#30455,#30456,#30457,#30458,#30459,
#30460,#30461,#30462,#30463,#30464,#30465,#30466,#30467,#30468,#30469,#30470,
#30471,#30472,#30473,#30474,#30475,#30476,#30477,#30478,#30479,#30480,#30481,
#30482,#30483,#30484,#30485,#30486,#30487,#30488,#30489,#30490,#30491,#30492,
#30493,#30494,#30495,#30496,#30497,#30498,#30499,#30500,#30501,#30502,#30503,
#30504,#30505,#30506,#30507,#30508,#30509,#30510,#30511,#30512,#30513,#30514,
#30515,#30516,#30517,#30518,#30519,#30520,#30521,#30522,#30523,#30524,#30525,
#30526,#30527,#30528,#30529,#30530,#30531,#30532,#30533,#30534,#30535,#30536,
#30537,#30538,#30539,#30540,#30541,#30542,#30543,#30544,#30545,#30546,#30547,
#30548,#30549,#30550,#30551,#30552,#30553,#30554,#30555,#30556,#30557,#30558,
#30559,#30560,#30561,#30562,#30563,#30564,#30565,#30566,#30567,#30568,#30569,
#30570,#30571,#30572,#30573,#30574,#30575,#30576,#30577,#30578,#30579,#30580,
#30581,#30582,#30583,#30584,#30585,#30586,#30587,#30588,#30589,#30590,#30591,
#30592,#30593,#30594,#30595,#30596,#30597,#30598,#30599,#30600,#30601,#30602,
#30603,#30604,#30605,#30606,#30607,#30608,#30609,#30610,#30611,#30612,#30613,
#30614,#30615,#30616,#30617,#30618,#30619,#30620,#30621,#30622,#30623,#30624,
#30625,#30626,#30627,#30628,#30629,#30630,#30631,#30632,#30633,#30634,#30635,
#30636,#30637,#30638,#30639,#30640,#30641,#30642,#30643,#30644,#30645,#30646,
#30647,#30648,#30649,#30650,#30651,#30652,#30653,#30654,#30655,#30656,#30657,
#30658,#30659,#30660,#30661,#30662,#30663,#30664,#30665,#30666,#30667,#30668,
#30669,#30670,#30671,#30672,#30673,#30674,#30675,#30676,#30677,#30678,#30679,
#30680,#30681,#30682,#30683,#30684,#30685),(#30686,#30687,#30688,#30689,
#30690,#30691,#30692,#30693,#30694,#30695,#30696,#30697,#30698,#30699,#30700,
#30701,#30702,#30703,#30704,#30705,#30706,#30707,#30708,#30709,#30710,#30711,
#30712,#30713,#30714,#30715,#30716,#30717,#30718,#30719,#30720,#30721,#30722,
#30723,#30724,#30725,#30726,#30727,#30728,#30729,#30730,#30731,#30732,#30733,
#30734,#30735,#30736,#30737,#30738,#30739,#30740,#30741,#30742,#30743,#30744,
#30745,#30746,#30747,#30748,#30749,#30750,#30751,#30752,#30753,#30754,#30755,
#30756,#30757,#30758,#30759,#30760,#30761,#30762,#30763,#30764,#30765,#30766,
#30767,#30768,#30769,#30770,#30771,#30772,#30773,#30774,#30775,#30776,#30777,
#30778,#30779,#30780,#30781,#30782,#30783,#30784,#30785,#30786,#30787,#30788,
#30789,#30790,#30791,#30792,#30793,#30794,#30795,#30796,#30797,#30798,#30799,
#30800,#30801,#30802,#30803,#30804,#30805,#30806,#30807,#30808,#30809,#30810,
#30811,#30812,#30813,#30814,#30815,#30816,#30817,#30818,#30819,#30820,#30821,
#30822,#30823,#30824,#30825,#30826,#30827,#30828,#30829,#30830,#30831,#30832,
#30833,#30834,#30835,#30836,#30837,#30838,#30839,#30840,#30841,#30842,#30843,
#30844,#30845,#30846,#30847,#30848,#30849,#30850,#30851,#30852,#30853,#30854,
#30855,#30856,#30857,#30858,#30859,#30860,#30861,#30862,#30863,#30864,#30865,
#30866,#30867,#30868,#30869,#30870,#30871,#30872,#30873,#30874,#30875,#30876,
#30877,#30878,#30879,#30880,#30881,#30882,#30883,#30884,#30885,#30886,#30887,
#30888,#30889,#30890,#30891,#30892,#30893,#30894,#30895,#30896,#30897,#30898,
#30899,#30900,#30901,#30902,#30903,#30904,#30905,#30906,#30907,#30908,#30909,
#30910,#30911,#30912,#30913,#30914,#30915,#30916,#30917,#30918,#30919,#30920,
#30921,#30922,#30923,#30924,#30925,#30926,#30927,#30928,#30929,#30930,#30931,
#30932,#30933,#30934,#30935,#30936,#30937,#30938,#30939,#30940,#30941,#30942,
#30943,#30944,#30945,#30946,#30947,#30948,#30949,#30950,#30951,#30952,#30953,
#30954,#30955,#30956,#30957,#30958,#30959,#30960,#30961,#30962,#30963,#30964,
#30965,#30966,#30967,#30968,#30969,#30970,#30971,#30972,#30973,#30974,#30975,
#30976,#30977,#30978,#30979,#30980,#30981,#30982,#30983,#30984,#30985,#30986,
#30987,#30988,#30989,#30990,#30991,#30992,#30993,#30994,#30995,#30996,#30997,
#30998,#30999,#31000,#31001,#31002,#31003,#31004,#31005,#31006,#31007,#31008,
#31009,#31010,#31011,#31012,#31013,#31014,#31015,#31016,#31017,#31018,#31019,
#31020,#31021,#31022,#31023,#31024,#31025,#31026,#31027,#31028,#31029,#31030,
#31031,#31032,#31033,#31034,#31035,#31036,#31037,#31038,#31039,#31040,#31041,
#31042,#31043,#31044,#31045,#31046,#31047,#31048,#31049,#31050,#31051,#31052,
#31053,#31054,#31055,#31056,#31057,#31058,#31059,#31060,#31061,#31062,#31063,
#31064,#31065,#31066,#31067,#31068,#31069,#31070,#31071,#31072,#31073,#31074,
#31075,#31076,#31077,#31078,#31079,#31080,#31081,#31082,#31083,#31084,#31085,
#31086,#31087,#31088,#31089,#31090,#31091,#31092,#31093,#31094,#31095,#31096,
#31097,#31098,#31099,#31100,#31101,#31102,#31103,#31104,#31105,#31106,#31107,
#31108,#31109,#31110,#31111,#31112,#31113,#31114,#31115,#31116,#31117,#31118,
#31119,#31120,#31121,#31122,#31123,#31124,#31125,#31126,#31127,#31128,#31129,
#31130,#31131,#31132,#31133,#31134,#31135,#31136,#31137,#31138,#31139,#31140,
#31141,#31142,#31143,#31144,#31145,#31146,#31147,#31148,#31149,#31150,#31151,
#31152,#31153,#31154,#31155,#31156,#31157,#31158,#31159,#31160,#31161,#31162,
#31163,#31164,#31165,#31166,#31167,#31168,#31169,#31170,#31171,#31172,#31173,
#31174,#31175,#31176,#31177,#31178,#31179,#31180,#31181,#31182,#31183)),
 .UNSPECIFIED.,.F.,.F.,.F.,(4,4),(4,1,1,1,1,1,1,1,1,1,1,1,1,1,1,1,1,1,1,
1,1,1,1,1,1,1,1,1,1,1,1,1,1,1,1,1,1,1,1,1,1,1,1,1,1,1,1,1,1,1,1,1,1,1,1,
1,1,1,1,1,1,1,1,1,1,1,1,1,1,1,1,1,1,1,1,1,1,1,1,1,1,1,1,1,1,1,1,1,1,1,1,
1,1,1,1,1,1,1,1,1,1,1,1,1,1,1,1,1,1,1,1,1,1,1,1,1,1,1,1,1,1,1,1,1,1,1,1,
1,1,1,1,1,1,1,1,1,1,1,1,1,1,1,1,1,1,1,1,1,1,1,1,1,1,1,1,1,1,1,1,1,1,1,1,
1,1,1,1,1,1,1,1,1,1,1,1,1,1,1,1,1,1,1,1,1,1,1,1,1,1,1,1,1,1,1,1,1,1,1,1,
1,1,1,1,1,1,1,1,1,1,1,1,1,1,1,1,1,1,1,1,1,1,1,1,1,1,1,1,1,1,1,1,1,1,1,1,
1,1,1,1,1,1,1,1,1,1,1,1,1,1,1,1,1,1,1,1,1,1,1,1,1,1,1,1,1,1,1,1,1,1,1,1,
1,1,1,1,1,1,1,1,1,1,1,1,1,1,1,1,1,1,1,1,1,1,1,1,1,1,1,1,1,1,1,1,1,1,1,1,
1,1,1,1,1,1,1,1,1,1,1,1,1,1,1,1,1,1,1,1,1,1,1,1,1,1,1,1,1,1,1,1,1,1,1,1,
1,1,1,1,1,1,1,1,1,1,1,1,1,1,1,1,1,1,1,1,1,1,1,1,1,1,1,1,1,1,1,1,1,1,1,1,
1,1,1,1,1,1,1,1,1,1,1,1,1,1,1,1,1,1,1,1,1,1,1,1,1,1,1,1,1,1,1,1,1,1,1,1,
1,1,1,1,1,1,1,1,1,1,1,1,1,1,1,1,1,1,1,1,1,1,1,1,1,1,1,1,1,1,1,1,1,1,1,1,
1,1,1,1,1,1,1,1,1,1,1,1,1,1,1,1,1,1,1,1,1,1,1,1,1,1,1,1,1,1,1,1,1,1,1,1,
1,1,1,1,1,1,1,1,4),(0.,0.184512097253587),(8.98171729021681,9.48139635699984,
9.98107542378286,10.4807544905659,10.9804335573489,11.4801126241319,11.979791690915,
12.479470757698,12.979149824481,13.478828891264,13.9785079580471,14.4781870248301,
14.9778660916131,15.4775451583961,15.9772242251791,16.4769032919622,16.9765823587452,
17.4762614255282,17.9759404923112,18.4756195590943,18.9752986258773,19.4749776926603,
19.9746567594433,20.4743358262264,20.9740148930094,21.4736939597924,21.9733730265754,
22.4730520933585,22.9727311601415,23.4724102269245,23.9720892937075,24.4717683604905,
24.9714474272736,25.4711264940566,25.9708055608396,26.4704846276226,26.9701636944057,
27.4698427611887,27.9695218279717,28.4692008947547,28.9688799615378,29.4685590283208,
29.9682380951038,30.4679171618868,30.9675962286699,31.4672752954529,31.9669543622359,
32.4666334290189,32.966312495802,33.465991562585,33.965670629368,34.465349696151,
34.965028762934,35.4647078297171,35.9643868965001,36.4640659632831,36.9637450300661,
37.4634240968492,37.9631031636322,38.4627822304152,38.9624612971982,39.4621403639813,
39.9618194307643,40.4614984975473,40.9611775643303,41.4608566311134,41.9605356978964,
42.4602147646794,42.9598938314624,43.4595728982454,43.9592519650285,44.4589310318115,
44.9586100985945,45.4582891653775,45.9579682321606,46.4576472989436,46.9573263657266,
47.4570054325096,47.9566844992927,48.4563635660757,48.9560426328587,49.4557216996417,
49.9554007664248,50.4550798332078,50.9547588999908,51.4544379667738,51.9541170335568,
52.4537961003399,52.9534751671229,53.4531542339059,53.9528333006889,54.452512367472,
54.952191434255,55.451870501038,55.951549567821,56.4512286346041,56.9509077013871,
57.4505867681701,57.9502658349531,58.4499449017362,58.9496239685192,59.9489821020852,
60.9483402356513,61.9476983692173,62.9470565027834,63.9464146363494,64.9457727699155,
65.9451309034815,66.9444890370476,67.9438471706136,68.9432053041797,69.9425634377457,
70.9419215713118,71.9412797048778,72.9406378384438,73.9399959720099,74.9393541055759,
75.938712239142,76.938070372708,77.9374285062741,78.9367866398401,79.9361447734062,
80.9355029069722,81.9348610405383,82.9342191741043,83.9335773076704,84.9329354412364,
85.9322935748025,86.9316517083685,87.9310098419346,88.9303679755006,89.9297261090666,
90.9290842426327,91.9284423761987,92.9278005097648,93.9271586433308,94.9265167768969,
95.9258749104629,96.925233044029,97.924591177595,98.9239493111611,99.9233074447271,
100.922665578293,101.922023711859,102.921381845425,103.920739978991,104.920098112557,
105.919456246123,106.918814379689,107.918172513255,108.917530646822,109.916888780388,
110.916246913954,111.91560504752,112.914963181086,113.914321314652,114.913679448218,
115.913037581784,116.91239571535,117.911753848916,118.911111982482,119.910470116048,
120.909828249614,121.90918638318,122.908544516746,123.907902650312,124.907260783878,
125.906618917444,126.90597705101,127.905335184576,128.904693318142,129.904051451709,
130.903409585275,131.902767718841,132.902125852407,133.901483985973,134.900842119539,
135.900200253105,136.899558386671,137.898916520237,138.898274653803,139.897632787369,
140.896990920935,141.896349054501,142.895707188067,143.895065321633,144.894423455199,
145.893781588765,146.893139722331,147.892497855897,148.891855989463,149.891214123029,
150.890572256596,151.889930390162,152.889288523728,153.888646657294,154.88800479086,
155.887362924426,156.886721057992,157.886079191558,158.885437325124,159.88479545869,
160.884153592256,161.883511725822,162.882869859388,163.882227992954,164.88158612652,
165.880944260086,166.880302393652,167.879660527218,168.879018660784,169.87837679435,
170.877734927916,171.877093061483,172.876451195049,173.875809328615,174.875167462181,
175.874525595747,176.873883729313,177.873241862879,178.872599996445,179.871958130011,
180.871316263577,181.870674397143,182.870032530709,183.869390664275,184.868748797841,
185.868106931407,186.867465064973,187.866823198539,188.866181332105,189.865539465671,
190.864897599237,191.864255732803,192.86361386637,193.862971999936,194.862330133502,
195.861688267068,196.861046400634,197.8604045342,198.859762667766,199.859120801332,
200.858478934898,201.857837068464,202.85719520203,203.856553335596,204.855911469162,
205.855269602728,206.854627736294,207.85398586986,208.853344003426,209.852702136992,
210.852060270558,211.851418404124,212.85077653769,213.850134671257,214.849492804823,
215.848850938389,216.848209071955,217.847567205521,218.846925339087,219.846283472653,
220.845641606219,221.844999739785,222.844357873351,223.843716006917,224.843074140483,
225.842432274049,226.841790407615,227.841148541181,228.840506674747,229.839864808313,
230.839222941879,231.838581075445,232.837939209011,233.837297342577,234.836655476144,
235.83601360971,236.835371743276,237.834729876842,238.834088010408,239.833446143974,
240.83280427754,241.832162411106,242.831520544672,243.830878678238,244.830236811804,
245.82959494537,246.828953078936,247.828311212502,248.827669346068,249.827027479634,
250.8263856132,251.825743746766,252.825101880332,253.824460013898,254.823818147464,
255.82317628103,256.822534414597,257.821892548163,258.821250681729,259.820608815295,
260.819966948861,261.819325082427,262.818683215993,263.818041349559,264.817399483125,
265.816757616691,266.816115750257,267.815473883823,268.814832017389,269.814190150955,
270.813548284521,271.812906418087,272.812264551653,273.811622685219,274.810980818785,
275.810338952351,276.809697085917,277.809055219484,278.80841335305,279.807771486616,
280.807129620182,281.806487753748,282.805845887314,283.80520402088,284.804562154446,
285.803920288012,286.803278421578,287.802636555144,288.80199468871,289.801352822276,
290.800710955842,291.800069089408,292.799427222974,293.79878535654,294.798143490106,
295.797501623672,296.796859757238,297.796217890804,298.795576024371,299.794934157937,
300.794292291503,301.793650425069,302.793008558635,303.792366692201,304.791724825767,
305.791082959333,306.790441092899,307.789799226465,308.789157360031,309.788515493597,
310.787873627163,311.787231760729,312.786589894295,313.785948027861,314.785306161427,
315.784664294993,316.784022428559,317.783380562125,318.782738695691,319.782096829258,
320.781454962824,321.78081309639,322.780171229956,323.779529363522,324.778887497088,
325.778245630654,326.77760376422,327.776961897786,328.776320031352,329.775678164918,
330.775036298484,331.77439443205,332.773752565616,333.773110699182,334.772468832748,
335.771826966314,336.77118509988,337.770543233446,338.769901367012,339.769259500578,
340.768617634145,341.767975767711,342.767333901277,343.766692034843,344.766050168409,
345.765408301975,346.764766435541,347.764124569107,348.763482702673,349.762840836239,
350.762198969805,351.761557103371,352.760915236937,353.760273370503,354.259952437286,
354.759631504069,355.259310570852,355.758989637635,356.258668704418,356.758347771201,
357.258026837984,357.757705904767,358.25738497155,358.757064038333,359.256743105116,
359.756422171899,360.256101238682,360.755780305465,361.255459372248,361.755138439031,
362.254817505815,362.754496572598,363.254175639381,363.753854706164,364.253533772947,
364.75321283973,365.252891906513,365.752570973296,366.252250040079,366.751929106862,
367.251608173645,367.751287240428,368.250966307211,368.750645373994,369.250324440777,
369.75000350756,370.249682574343,370.749361641126,371.249040707909,371.748719774692,
372.248398841475,372.748077908258,373.247756975041,373.747436041824,374.247115108607,
374.74679417539,375.246473242173,375.746152308956,376.245831375739,376.745510442522,
377.245189509305,377.744868576088,378.244547642871,378.744226709654,379.243905776437,
379.74358484322,380.243263910003,380.742942976786,381.242622043569,381.742301110352,
382.241980177135,382.741659243918,383.241338310702,383.741017377485,384.240696444268,
384.740375511051,385.240054577834,385.739733644617,386.2394127114,386.739091778183,
387.238770844966,387.738449911749,388.238128978532,388.737808045315,389.237487112098,
389.737166178881,390.236845245664,390.736524312447,391.23620337923,391.735882446013,
392.235561512796,392.735240579579,393.234919646362,393.734598713145,394.234277779928,
394.733956846711,395.233635913494,395.733314980277,396.23299404706,396.732673113843,
397.232352180626,397.732031247409,398.231710314192,398.731389380975,399.231068447758,
399.730747514541,400.230426581324,400.730105648107,401.22978471489,401.729463781673,
402.229142848456,402.728821915239,403.228500982022,403.728180048805),
 .UNSPECIFIED.);
#14=B_SPLINE_SURFACE_WITH_KNOTS('',3,3,((#31277,#31278,#31279,#31280,#31281,
#31282,#31283,#31284,#31285,#31286,#31287,#31288,#31289,#31290,#31291,#31292,
#31293,#31294,#31295,#31296,#31297,#31298,#31299,#31300,#31301,#31302,#31303,
#31304,#31305,#31306,#31307,#31308,#31309,#31310,#31311,#31312,#31313,#31314,
#31315,#31316,#31317,#31318,#31319,#31320,#31321,#31322,#31323,#31324,#31325,
#31326,#31327,#31328,#31329,#31330,#31331,#31332,#31333,#31334,#31335,#31336,
#31337,#31338,#31339,#31340,#31341,#31342,#31343,#31344,#31345,#31346,#31347,
#31348,#31349,#31350,#31351,#31352,#31353,#31354,#31355,#31356,#31357,#31358,
#31359,#31360,#31361,#31362,#31363,#31364,#31365,#31366,#31367,#31368,#31369,
#31370,#31371,#31372,#31373,#31374,#31375,#31376,#31377,#31378,#31379,#31380,
#31381,#31382,#31383,#31384,#31385,#31386,#31387,#31388,#31389,#31390,#31391,
#31392,#31393,#31394,#31395,#31396,#31397,#31398,#31399,#31400,#31401,#31402,
#31403,#31404,#31405,#31406,#31407,#31408,#31409,#31410,#31411,#31412,#31413,
#31414,#31415,#31416,#31417,#31418,#31419,#31420,#31421,#31422,#31423,#31424,
#31425,#31426,#31427,#31428,#31429,#31430,#31431,#31432,#31433,#31434,#31435,
#31436,#31437,#31438,#31439,#31440,#31441,#31442,#31443,#31444,#31445,#31446,
#31447,#31448,#31449,#31450,#31451,#31452,#31453,#31454,#31455,#31456,#31457,
#31458,#31459,#31460,#31461,#31462,#31463,#31464,#31465,#31466,#31467,#31468,
#31469,#31470,#31471,#31472,#31473,#31474,#31475,#31476,#31477,#31478,#31479,
#31480,#31481,#31482,#31483,#31484,#31485,#31486,#31487,#31488,#31489,#31490,
#31491,#31492,#31493,#31494,#31495,#31496,#31497,#31498,#31499,#31500,#31501,
#31502,#31503,#31504,#31505,#31506,#31507,#31508,#31509,#31510,#31511,#31512,
#31513,#31514,#31515,#31516,#31517,#31518,#31519,#31520,#31521,#31522,#31523,
#31524,#31525,#31526,#31527,#31528,#31529,#31530,#31531,#31532,#31533,#31534,
#31535,#31536,#31537,#31538,#31539,#31540,#31541,#31542,#31543,#31544,#31545,
#31546,#31547,#31548,#31549,#31550,#31551,#31552,#31553,#31554,#31555,#31556,
#31557,#31558,#31559,#31560,#31561,#31562,#31563,#31564,#31565,#31566,#31567,
#31568,#31569,#31570,#31571,#31572,#31573,#31574,#31575,#31576,#31577,#31578,
#31579,#31580,#31581,#31582,#31583,#31584,#31585,#31586,#31587,#31588,#31589,
#31590,#31591,#31592,#31593,#31594,#31595,#31596,#31597,#31598,#31599,#31600,
#31601,#31602,#31603,#31604,#31605,#31606,#31607,#31608,#31609,#31610,#31611,
#31612,#31613,#31614,#31615,#31616,#31617,#31618,#31619,#31620,#31621,#31622,
#31623,#31624,#31625,#31626,#31627,#31628,#31629,#31630,#31631,#31632,#31633,
#31634,#31635,#31636,#31637,#31638,#31639,#31640,#31641,#31642,#31643,#31644,
#31645,#31646,#31647,#31648,#31649,#31650,#31651,#31652,#31653,#31654,#31655,
#31656,#31657,#31658,#31659,#31660,#31661,#31662,#31663,#31664,#31665,#31666,
#31667,#31668,#31669,#31670,#31671,#31672,#31673,#31674,#31675,#31676,#31677,
#31678,#31679,#31680,#31681,#31682,#31683,#31684,#31685,#31686,#31687,#31688,
#31689,#31690,#31691,#31692,#31693,#31694,#31695,#31696,#31697,#31698,#31699,
#31700,#31701,#31702,#31703,#31704,#31705,#31706,#31707,#31708,#31709,#31710,
#31711,#31712,#31713,#31714,#31715,#31716,#31717,#31718,#31719,#31720,#31721,
#31722,#31723,#31724,#31725,#31726,#31727,#31728,#31729,#31730,#31731,#31732,
#31733,#31734,#31735,#31736,#31737,#31738,#31739,#31740,#31741,#31742,#31743,
#31744,#31745,#31746,#31747,#31748,#31749,#31750,#31751,#31752,#31753,#31754,
#31755,#31756,#31757,#31758,#31759,#31760,#31761,#31762,#31763,#31764,#31765,
#31766,#31767,#31768,#31769,#31770,#31771,#31772,#31773,#31774),(#31775,
#31776,#31777,#31778,#31779,#31780,#31781,#31782,#31783,#31784,#31785,#31786,
#31787,#31788,#31789,#31790,#31791,#31792,#31793,#31794,#31795,#31796,#31797,
#31798,#31799,#31800,#31801,#31802,#31803,#31804,#31805,#31806,#31807,#31808,
#31809,#31810,#31811,#31812,#31813,#31814,#31815,#31816,#31817,#31818,#31819,
#31820,#31821,#31822,#31823,#31824,#31825,#31826,#31827,#31828,#31829,#31830,
#31831,#31832,#31833,#31834,#31835,#31836,#31837,#31838,#31839,#31840,#31841,
#31842,#31843,#31844,#31845,#31846,#31847,#31848,#31849,#31850,#31851,#31852,
#31853,#31854,#31855,#31856,#31857,#31858,#31859,#31860,#31861,#31862,#31863,
#31864,#31865,#31866,#31867,#31868,#31869,#31870,#31871,#31872,#31873,#31874,
#31875,#31876,#31877,#31878,#31879,#31880,#31881,#31882,#31883,#31884,#31885,
#31886,#31887,#31888,#31889,#31890,#31891,#31892,#31893,#31894,#31895,#31896,
#31897,#31898,#31899,#31900,#31901,#31902,#31903,#31904,#31905,#31906,#31907,
#31908,#31909,#31910,#31911,#31912,#31913,#31914,#31915,#31916,#31917,#31918,
#31919,#31920,#31921,#31922,#31923,#31924,#31925,#31926,#31927,#31928,#31929,
#31930,#31931,#31932,#31933,#31934,#31935,#31936,#31937,#31938,#31939,#31940,
#31941,#31942,#31943,#31944,#31945,#31946,#31947,#31948,#31949,#31950,#31951,
#31952,#31953,#31954,#31955,#31956,#31957,#31958,#31959,#31960,#31961,#31962,
#31963,#31964,#31965,#31966,#31967,#31968,#31969,#31970,#31971,#31972,#31973,
#31974,#31975,#31976,#31977,#31978,#31979,#31980,#31981,#31982,#31983,#31984,
#31985,#31986,#31987,#31988,#31989,#31990,#31991,#31992,#31993,#31994,#31995,
#31996,#31997,#31998,#31999,#32000,#32001,#32002,#32003,#32004,#32005,#32006,
#32007,#32008,#32009,#32010,#32011,#32012,#32013,#32014,#32015,#32016,#32017,
#32018,#32019,#32020,#32021,#32022,#32023,#32024,#32025,#32026,#32027,#32028,
#32029,#32030,#32031,#32032,#32033,#32034,#32035,#32036,#32037,#32038,#32039,
#32040,#32041,#32042,#32043,#32044,#32045,#32046,#32047,#32048,#32049,#32050,
#32051,#32052,#32053,#32054,#32055,#32056,#32057,#32058,#32059,#32060,#32061,
#32062,#32063,#32064,#32065,#32066,#32067,#32068,#32069,#32070,#32071,#32072,
#32073,#32074,#32075,#32076,#32077,#32078,#32079,#32080,#32081,#32082,#32083,
#32084,#32085,#32086,#32087,#32088,#32089,#32090,#32091,#32092,#32093,#32094,
#32095,#32096,#32097,#32098,#32099,#32100,#32101,#32102,#32103,#32104,#32105,
#32106,#32107,#32108,#32109,#32110,#32111,#32112,#32113,#32114,#32115,#32116,
#32117,#32118,#32119,#32120,#32121,#32122,#32123,#32124,#32125,#32126,#32127,
#32128,#32129,#32130,#32131,#32132,#32133,#32134,#32135,#32136,#32137,#32138,
#32139,#32140,#32141,#32142,#32143,#32144,#32145,#32146,#32147,#32148,#32149,
#32150,#32151,#32152,#32153,#32154,#32155,#32156,#32157,#32158,#32159,#32160,
#32161,#32162,#32163,#32164,#32165,#32166,#32167,#32168,#32169,#32170,#32171,
#32172,#32173,#32174,#32175,#32176,#32177,#32178,#32179,#32180,#32181,#32182,
#32183,#32184,#32185,#32186,#32187,#32188,#32189,#32190,#32191,#32192,#32193,
#32194,#32195,#32196,#32197,#32198,#32199,#32200,#32201,#32202,#32203,#32204,
#32205,#32206,#32207,#32208,#32209,#32210,#32211,#32212,#32213,#32214,#32215,
#32216,#32217,#32218,#32219,#32220,#32221,#32222,#32223,#32224,#32225,#32226,
#32227,#32228,#32229,#32230,#32231,#32232,#32233,#32234,#32235,#32236,#32237,
#32238,#32239,#32240,#32241,#32242,#32243,#32244,#32245,#32246,#32247,#32248,
#32249,#32250,#32251,#32252,#32253,#32254,#32255,#32256,#32257,#32258,#32259,
#32260,#32261,#32262,#32263,#32264,#32265,#32266,#32267,#32268,#32269,#32270,
#32271,#32272),(#32273,#32274,#32275,#32276,#32277,#32278,#32279,#32280,
#32281,#32282,#32283,#32284,#32285,#32286,#32287,#32288,#32289,#32290,#32291,
#32292,#32293,#32294,#32295,#32296,#32297,#32298,#32299,#32300,#32301,#32302,
#32303,#32304,#32305,#32306,#32307,#32308,#32309,#32310,#32311,#32312,#32313,
#32314,#32315,#32316,#32317,#32318,#32319,#32320,#32321,#32322,#32323,#32324,
#32325,#32326,#32327,#32328,#32329,#32330,#32331,#32332,#32333,#32334,#32335,
#32336,#32337,#32338,#32339,#32340,#32341,#32342,#32343,#32344,#32345,#32346,
#32347,#32348,#32349,#32350,#32351,#32352,#32353,#32354,#32355,#32356,#32357,
#32358,#32359,#32360,#32361,#32362,#32363,#32364,#32365,#32366,#32367,#32368,
#32369,#32370,#32371,#32372,#32373,#32374,#32375,#32376,#32377,#32378,#32379,
#32380,#32381,#32382,#32383,#32384,#32385,#32386,#32387,#32388,#32389,#32390,
#32391,#32392,#32393,#32394,#32395,#32396,#32397,#32398,#32399,#32400,#32401,
#32402,#32403,#32404,#32405,#32406,#32407,#32408,#32409,#32410,#32411,#32412,
#32413,#32414,#32415,#32416,#32417,#32418,#32419,#32420,#32421,#32422,#32423,
#32424,#32425,#32426,#32427,#32428,#32429,#32430,#32431,#32432,#32433,#32434,
#32435,#32436,#32437,#32438,#32439,#32440,#32441,#32442,#32443,#32444,#32445,
#32446,#32447,#32448,#32449,#32450,#32451,#32452,#32453,#32454,#32455,#32456,
#32457,#32458,#32459,#32460,#32461,#32462,#32463,#32464,#32465,#32466,#32467,
#32468,#32469,#32470,#32471,#32472,#32473,#32474,#32475,#32476,#32477,#32478,
#32479,#32480,#32481,#32482,#32483,#32484,#32485,#32486,#32487,#32488,#32489,
#32490,#32491,#32492,#32493,#32494,#32495,#32496,#32497,#32498,#32499,#32500,
#32501,#32502,#32503,#32504,#32505,#32506,#32507,#32508,#32509,#32510,#32511,
#32512,#32513,#32514,#32515,#32516,#32517,#32518,#32519,#32520,#32521,#32522,
#32523,#32524,#32525,#32526,#32527,#32528,#32529,#32530,#32531,#32532,#32533,
#32534,#32535,#32536,#32537,#32538,#32539,#32540,#32541,#32542,#32543,#32544,
#32545,#32546,#32547,#32548,#32549,#32550,#32551,#32552,#32553,#32554,#32555,
#32556,#32557,#32558,#32559,#32560,#32561,#32562,#32563,#32564,#32565,#32566,
#32567,#32568,#32569,#32570,#32571,#32572,#32573,#32574,#32575,#32576,#32577,
#32578,#32579,#32580,#32581,#32582,#32583,#32584,#32585,#32586,#32587,#32588,
#32589,#32590,#32591,#32592,#32593,#32594,#32595,#32596,#32597,#32598,#32599,
#32600,#32601,#32602,#32603,#32604,#32605,#32606,#32607,#32608,#32609,#32610,
#32611,#32612,#32613,#32614,#32615,#32616,#32617,#32618,#32619,#32620,#32621,
#32622,#32623,#32624,#32625,#32626,#32627,#32628,#32629,#32630,#32631,#32632,
#32633,#32634,#32635,#32636,#32637,#32638,#32639,#32640,#32641,#32642,#32643,
#32644,#32645,#32646,#32647,#32648,#32649,#32650,#32651,#32652,#32653,#32654,
#32655,#32656,#32657,#32658,#32659,#32660,#32661,#32662,#32663,#32664,#32665,
#32666,#32667,#32668,#32669,#32670,#32671,#32672,#32673,#32674,#32675,#32676,
#32677,#32678,#32679,#32680,#32681,#32682,#32683,#32684,#32685,#32686,#32687,
#32688,#32689,#32690,#32691,#32692,#32693,#32694,#32695,#32696,#32697,#32698,
#32699,#32700,#32701,#32702,#32703,#32704,#32705,#32706,#32707,#32708,#32709,
#32710,#32711,#32712,#32713,#32714,#32715,#32716,#32717,#32718,#32719,#32720,
#32721,#32722,#32723,#32724,#32725,#32726,#32727,#32728,#32729,#32730,#32731,
#32732,#32733,#32734,#32735,#32736,#32737,#32738,#32739,#32740,#32741,#32742,
#32743,#32744,#32745,#32746,#32747,#32748,#32749,#32750,#32751,#32752,#32753,
#32754,#32755,#32756,#32757,#32758,#32759,#32760,#32761,#32762,#32763,#32764,
#32765,#32766,#32767,#32768,#32769,#32770),(#32771,#32772,#32773,#32774,
#32775,#32776,#32777,#32778,#32779,#32780,#32781,#32782,#32783,#32784,#32785,
#32786,#32787,#32788,#32789,#32790,#32791,#32792,#32793,#32794,#32795,#32796,
#32797,#32798,#32799,#32800,#32801,#32802,#32803,#32804,#32805,#32806,#32807,
#32808,#32809,#32810,#32811,#32812,#32813,#32814,#32815,#32816,#32817,#32818,
#32819,#32820,#32821,#32822,#32823,#32824,#32825,#32826,#32827,#32828,#32829,
#32830,#32831,#32832,#32833,#32834,#32835,#32836,#32837,#32838,#32839,#32840,
#32841,#32842,#32843,#32844,#32845,#32846,#32847,#32848,#32849,#32850,#32851,
#32852,#32853,#32854,#32855,#32856,#32857,#32858,#32859,#32860,#32861,#32862,
#32863,#32864,#32865,#32866,#32867,#32868,#32869,#32870,#32871,#32872,#32873,
#32874,#32875,#32876,#32877,#32878,#32879,#32880,#32881,#32882,#32883,#32884,
#32885,#32886,#32887,#32888,#32889,#32890,#32891,#32892,#32893,#32894,#32895,
#32896,#32897,#32898,#32899,#32900,#32901,#32902,#32903,#32904,#32905,#32906,
#32907,#32908,#32909,#32910,#32911,#32912,#32913,#32914,#32915,#32916,#32917,
#32918,#32919,#32920,#32921,#32922,#32923,#32924,#32925,#32926,#32927,#32928,
#32929,#32930,#32931,#32932,#32933,#32934,#32935,#32936,#32937,#32938,#32939,
#32940,#32941,#32942,#32943,#32944,#32945,#32946,#32947,#32948,#32949,#32950,
#32951,#32952,#32953,#32954,#32955,#32956,#32957,#32958,#32959,#32960,#32961,
#32962,#32963,#32964,#32965,#32966,#32967,#32968,#32969,#32970,#32971,#32972,
#32973,#32974,#32975,#32976,#32977,#32978,#32979,#32980,#32981,#32982,#32983,
#32984,#32985,#32986,#32987,#32988,#32989,#32990,#32991,#32992,#32993,#32994,
#32995,#32996,#32997,#32998,#32999,#33000,#33001,#33002,#33003,#33004,#33005,
#33006,#33007,#33008,#33009,#33010,#33011,#33012,#33013,#33014,#33015,#33016,
#33017,#33018,#33019,#33020,#33021,#33022,#33023,#33024,#33025,#33026,#33027,
#33028,#33029,#33030,#33031,#33032,#33033,#33034,#33035,#33036,#33037,#33038,
#33039,#33040,#33041,#33042,#33043,#33044,#33045,#33046,#33047,#33048,#33049,
#33050,#33051,#33052,#33053,#33054,#33055,#33056,#33057,#33058,#33059,#33060,
#33061,#33062,#33063,#33064,#33065,#33066,#33067,#33068,#33069,#33070,#33071,
#33072,#33073,#33074,#33075,#33076,#33077,#33078,#33079,#33080,#33081,#33082,
#33083,#33084,#33085,#33086,#33087,#33088,#33089,#33090,#33091,#33092,#33093,
#33094,#33095,#33096,#33097,#33098,#33099,#33100,#33101,#33102,#33103,#33104,
#33105,#33106,#33107,#33108,#33109,#33110,#33111,#33112,#33113,#33114,#33115,
#33116,#33117,#33118,#33119,#33120,#33121,#33122,#33123,#33124,#33125,#33126,
#33127,#33128,#33129,#33130,#33131,#33132,#33133,#33134,#33135,#33136,#33137,
#33138,#33139,#33140,#33141,#33142,#33143,#33144,#33145,#33146,#33147,#33148,
#33149,#33150,#33151,#33152,#33153,#33154,#33155,#33156,#33157,#33158,#33159,
#33160,#33161,#33162,#33163,#33164,#33165,#33166,#33167,#33168,#33169,#33170,
#33171,#33172,#33173,#33174,#33175,#33176,#33177,#33178,#33179,#33180,#33181,
#33182,#33183,#33184,#33185,#33186,#33187,#33188,#33189,#33190,#33191,#33192,
#33193,#33194,#33195,#33196,#33197,#33198,#33199,#33200,#33201,#33202,#33203,
#33204,#33205,#33206,#33207,#33208,#33209,#33210,#33211,#33212,#33213,#33214,
#33215,#33216,#33217,#33218,#33219,#33220,#33221,#33222,#33223,#33224,#33225,
#33226,#33227,#33228,#33229,#33230,#33231,#33232,#33233,#33234,#33235,#33236,
#33237,#33238,#33239,#33240,#33241,#33242,#33243,#33244,#33245,#33246,#33247,
#33248,#33249,#33250,#33251,#33252,#33253,#33254,#33255,#33256,#33257,#33258,
#33259,#33260,#33261,#33262,#33263,#33264,#33265,#33266,#33267,#33268)),
 .UNSPECIFIED.,.F.,.F.,.F.,(4,4),(4,1,1,1,1,1,1,1,1,1,1,1,1,1,1,1,1,1,1,
1,1,1,1,1,1,1,1,1,1,1,1,1,1,1,1,1,1,1,1,1,1,1,1,1,1,1,1,1,1,1,1,1,1,1,1,
1,1,1,1,1,1,1,1,1,1,1,1,1,1,1,1,1,1,1,1,1,1,1,1,1,1,1,1,1,1,1,1,1,1,1,1,
1,1,1,1,1,1,1,1,1,1,1,1,1,1,1,1,1,1,1,1,1,1,1,1,1,1,1,1,1,1,1,1,1,1,1,1,
1,1,1,1,1,1,1,1,1,1,1,1,1,1,1,1,1,1,1,1,1,1,1,1,1,1,1,1,1,1,1,1,1,1,1,1,
1,1,1,1,1,1,1,1,1,1,1,1,1,1,1,1,1,1,1,1,1,1,1,1,1,1,1,1,1,1,1,1,1,1,1,1,
1,1,1,1,1,1,1,1,1,1,1,1,1,1,1,1,1,1,1,1,1,1,1,1,1,1,1,1,1,1,1,1,1,1,1,1,
1,1,1,1,1,1,1,1,1,1,1,1,1,1,1,1,1,1,1,1,1,1,1,1,1,1,1,1,1,1,1,1,1,1,1,1,
1,1,1,1,1,1,1,1,1,1,1,1,1,1,1,1,1,1,1,1,1,1,1,1,1,1,1,1,1,1,1,1,1,1,1,1,
1,1,1,1,1,1,1,1,1,1,1,1,1,1,1,1,1,1,1,1,1,1,1,1,1,1,1,1,1,1,1,1,1,1,1,1,
1,1,1,1,1,1,1,1,1,1,1,1,1,1,1,1,1,1,1,1,1,1,1,1,1,1,1,1,1,1,1,1,1,1,1,1,
1,1,1,1,1,1,1,1,1,1,1,1,1,1,1,1,1,1,1,1,1,1,1,1,1,1,1,1,1,1,1,1,1,1,1,1,
1,1,1,1,1,1,1,1,1,1,1,1,1,1,1,1,1,1,1,1,1,1,1,1,1,1,1,1,1,1,1,1,1,1,1,1,
1,1,1,1,1,1,1,1,1,1,1,1,1,1,1,1,1,1,1,1,1,1,1,1,1,1,1,1,1,1,1,1,1,1,1,1,
1,1,1,1,1,1,1,1,4),(0.,0.184512097253587),(12.0092477762453,12.5089268430284,
13.0086059098114,13.5082849765944,14.0079640433774,14.5076431101605,15.0073221769435,
15.5070012437265,16.0066803105095,16.5063593772925,17.0060384440756,17.5057175108586,
18.0053965776416,18.5050756444246,19.0047547112077,19.5044337779907,20.0041128447737,
20.5037919115567,21.0034709783398,21.5031500451228,22.0028291119058,22.5025081786888,
23.0021872454719,23.5018663122549,24.0015453790379,24.5012244458209,25.0009035126039,
25.500582579387,26.00026164617,26.499940712953,26.999619779736,27.4992988465191,
27.9989779133021,28.4986569800851,28.9983360468681,29.4980151136512,29.9976941804342,
30.4973732472172,30.9970523140002,31.4967313807832,31.9964104475663,32.4960895143493,
32.9957685811323,33.4954476479153,33.9951267146984,34.4948057814814,34.9944848482644,
35.4941639150474,35.9938429818305,36.4935220486135,36.9932011153965,37.4928801821795,
37.9925592489626,38.4922383157456,38.9919173825286,39.4915964493116,39.9912755160946,
40.4909545828777,40.9906336496607,41.4903127164437,41.9899917832267,42.4896708500098,
42.9893499167928,43.4890289835758,43.9887080503588,44.4883871171419,44.9880661839249,
45.4877452507079,45.9874243174909,46.4871033842739,46.986782451057,47.48646151784,
47.986140584623,48.485819651406,48.9854987181891,49.4851777849721,49.9848568517551,
50.4845359185381,50.9842149853212,51.4838940521042,51.9835731188872,52.4832521856702,
52.9829312524532,53.4826103192363,53.9822893860193,54.4819684528023,54.9816475195853,
55.4813265863684,55.9810056531514,56.4806847199344,56.9803637867174,57.4800428535005,
57.9797219202835,58.4794009870665,58.9790800538495,59.4787591206325,59.9784381874156,
60.4781172541986,60.9777963209816,61.4774753877646,61.9771544545477,62.9765125881137,
63.9758707216798,64.9752288552458,65.9745869888119,66.9739451223779,67.9733032559439,
68.97266138951,69.972019523076,70.9713776566421,71.9707357902081,72.9700939237742,
73.9694520573402,74.9688101909063,75.9681683244723,76.9675264580384,77.9668845916044,
78.9662427251705,79.9656008587365,80.9649589923026,81.9643171258686,82.9636752594347,
83.9630333930007,84.9623915265667,85.9617496601328,86.9611077936988,87.9604659272649,
88.9598240608309,89.959182194397,90.958540327963,91.9578984615291,92.9572565950951,
93.9566147286612,94.9559728622272,95.9553309957932,96.9546891293593,97.9540472629253,
98.9534053964914,99.9527635300574,100.952121663623,101.95147979719,102.950837930756,
103.950196064322,104.949554197888,105.948912331454,106.94827046502,107.947628598586,
108.946986732152,109.946344865718,110.945702999284,111.94506113285,112.944419266416,
113.943777399982,114.943135533548,115.942493667114,116.94185180068,117.941209934246,
118.940568067812,119.939926201378,120.939284334944,121.93864246851,122.938000602077,
123.937358735643,124.936716869209,125.936075002775,126.935433136341,127.934791269907,
128.934149403473,129.933507537039,130.932865670605,131.932223804171,132.931581937737,
133.930940071303,134.930298204869,135.929656338435,136.929014472001,137.928372605567,
138.927730739133,139.927088872699,140.926447006265,141.925805139831,142.925163273397,
143.924521406963,144.92387954053,145.923237674096,146.922595807662,147.921953941228,
148.921312074794,149.92067020836,150.920028341926,151.919386475492,152.918744609058,
153.918102742624,154.91746087619,155.916819009756,156.916177143322,157.915535276888,
158.914893410454,159.91425154402,160.913609677586,161.912967811152,162.912325944718,
163.911684078284,164.91104221185,165.910400345416,166.909758478983,167.909116612549,
168.908474746115,169.907832879681,170.907191013247,171.906549146813,172.905907280379,
173.905265413945,174.904623547511,175.903981681077,176.903339814643,177.902697948209,
178.902056081775,179.901414215341,180.900772348907,181.900130482473,182.899488616039,
183.898846749605,184.898204883171,185.897563016737,186.896921150303,187.89627928387,
188.895637417436,189.894995551002,190.894353684568,191.893711818134,192.8930699517,
193.892428085266,194.891786218832,195.891144352398,196.890502485964,197.88986061953,
198.889218753096,199.888576886662,200.887935020228,201.887293153794,202.88665128736,
203.886009420926,204.885367554492,205.884725688058,206.884083821624,207.88344195519,
208.882800088756,209.882158222323,210.881516355889,211.880874489455,212.880232623021,
213.879590756587,214.878948890153,215.878307023719,216.877665157285,217.877023290851,
218.876381424417,219.875739557983,220.875097691549,221.874455825115,222.873813958681,
223.873172092247,224.872530225813,225.871888359379,226.871246492945,227.870604626511,
228.869962760077,229.869320893643,230.86867902721,231.868037160776,232.867395294342,
233.866753427908,234.866111561474,235.86546969504,236.864827828606,237.864185962172,
238.863544095738,239.862902229304,240.86226036287,241.861618496436,242.860976630002,
243.860334763568,244.859692897134,245.8590510307,246.858409164266,247.857767297832,
248.857125431398,249.856483564964,250.85584169853,251.855199832097,252.854557965663,
253.853916099229,254.853274232795,255.852632366361,256.851990499927,257.851348633493,
258.850706767059,259.850064900625,260.849423034191,261.848781167757,262.848139301323,
263.847497434889,264.846855568455,265.846213702021,266.845571835587,267.844929969153,
268.844288102719,269.843646236285,270.843004369851,271.842362503417,272.841720636983,
273.84107877055,274.840436904116,275.839795037682,276.839153171248,277.838511304814,
278.83786943838,279.837227571946,280.836585705512,281.835943839078,282.835301972644,
283.83466010621,284.834018239776,285.833376373342,286.832734506908,287.832092640474,
288.83145077404,289.830808907606,290.830167041172,291.829525174738,292.828883308304,
293.82824144187,294.827599575437,295.826957709003,296.826315842569,297.825673976135,
298.825032109701,299.824390243267,300.823748376833,301.823106510399,302.822464643965,
303.821822777531,304.821180911097,305.820539044663,306.819897178229,307.819255311795,
308.818613445361,309.817971578927,310.817329712493,311.816687846059,312.816045979625,
313.815404113191,314.814762246757,315.814120380323,316.81347851389,317.812836647456,
318.812194781022,319.811552914588,320.810911048154,321.81026918172,322.809627315286,
323.808985448852,324.808343582418,325.807701715984,326.80705984955,327.806417983116,
328.805776116682,329.805134250248,330.804492383814,331.80385051738,332.803208650946,
333.802566784512,334.801924918078,335.801283051644,336.80064118521,337.799999318776,
338.799357452343,339.798715585909,340.798073719475,341.797431853041,342.796789986607,
343.796148120173,344.795506253739,345.794864387305,346.794222520871,347.793580654437,
348.792938788003,349.792296921569,350.791655055135,351.791013188701,352.790371322267,
353.789729455833,354.789087589399,355.788445722965,356.787803856531,357.287482923314,
357.787161990097,358.28684105688,358.786520123663,359.286199190446,359.78587825723,
360.285557324013,360.785236390796,361.284915457579,361.784594524362,362.284273591145,
362.783952657928,363.283631724711,363.783310791494,364.282989858277,364.78266892506,
365.282347991843,365.782027058626,366.281706125409,366.781385192192,367.281064258975,
367.780743325758,368.280422392541,368.780101459324,369.279780526107,369.77945959289,
370.279138659673,370.778817726456,371.278496793239,371.778175860022,372.277854926805,
372.777533993588,373.277213060371,373.776892127154,374.276571193937,374.77625026072,
375.275929327503,375.775608394286,376.275287461069,376.774966527852,377.274645594635,
377.774324661418,378.274003728201,378.773682794984,379.273361861767,379.77304092855,
380.272719995333,380.772399062117,381.2720781289,381.771757195683,382.271436262466,
382.771115329249,383.270794396032,383.770473462815,384.270152529598,384.769831596381,
385.269510663164,385.769189729947,386.26886879673,386.768547863513,387.268226930296,
387.767905997079,388.267585063862,388.767264130645,389.266943197428,389.766622264211,
390.266301330994,390.765980397777,391.26565946456,391.765338531343,392.265017598126,
392.764696664909,393.264375731692,393.764054798475,394.263733865258,394.763412932041,
395.263091998824,395.762771065607,396.26245013239,396.762129199173,397.261808265956,
397.761487332739,398.261166399522,398.760845466305,399.260524533088,399.760203599871,
400.259882666654,400.759561733437,401.25924080022,401.758919867003,402.258598933787,
402.75827800057,403.257957067353,403.757636134136,404.257315200919,404.756994267702,
405.256673334485,405.756352401268,406.256031468051,406.755710534834),
 .UNSPECIFIED.);
#15=ORIENTED_CLOSED_SHELL('',*,#13047,.F.);
#16=ORIENTED_CLOSED_SHELL('',*,#13056,.F.);
#17=ORIENTED_CLOSED_SHELL('',*,#13060,.F.);
#18=ORIENTED_CLOSED_SHELL('',*,#13062,.F.);
#19=ORIENTED_CLOSED_SHELL('',*,#13073,.F.);
#20=BREP_WITH_VOIDS('Body1',#13048,(#15));
#21=BREP_WITH_VOIDS('Body1',#13057,(#16));
#22=BREP_WITH_VOIDS('Body1',#13059,(#17));
#23=BREP_WITH_VOIDS('Body1',#13061,(#18));
#24=BREP_WITH_VOIDS('Body1',#13072,(#19));
#25=ELLIPSE('',#14185,0.299389011154384,0.2117);
#26=ELLIPSE('',#14190,0.299389011154384,0.2117);
#27=ITEM_DEFINED_TRANSFORMATION($,$,#13872,#13994);
#28=ITEM_DEFINED_TRANSFORMATION($,$,#13892,#13995);
#29=ITEM_DEFINED_TRANSFORMATION($,$,#13912,#13996);
#30=ITEM_DEFINED_TRANSFORMATION($,$,#13927,#13997);
#31=ITEM_DEFINED_TRANSFORMATION($,$,#13977,#13998);
#32=ITEM_DEFINED_TRANSFORMATION($,$,#14000,#14128);
#33=ITEM_DEFINED_TRANSFORMATION($,$,#14020,#14129);
#34=ITEM_DEFINED_TRANSFORMATION($,$,#14040,#14130);
#35=ITEM_DEFINED_TRANSFORMATION($,$,#14057,#14131);
#36=ITEM_DEFINED_TRANSFORMATION($,$,#14111,#14132);
#37=ITEM_DEFINED_TRANSFORMATION($,$,#14325,#14386);
#38=ITEM_DEFINED_TRANSFORMATION($,$,#14364,#14387);
#39=ITEM_DEFINED_TRANSFORMATION($,$,#14375,#14388);
#40=ITEM_DEFINED_TRANSFORMATION($,$,#14236,#14525);
#41=ITEM_DEFINED_TRANSFORMATION($,$,#14255,#14526);
#42=ITEM_DEFINED_TRANSFORMATION($,$,#14286,#14527);
#43=ITEM_DEFINED_TRANSFORMATION($,$,#14324,#14528);
#44=ITEM_DEFINED_TRANSFORMATION($,$,#14389,#14529);
#45=ITEM_DEFINED_TRANSFORMATION($,$,#14400,#14530);
#46=ITEM_DEFINED_TRANSFORMATION($,$,#14389,#14531);
#47=ITEM_DEFINED_TRANSFORMATION($,$,#14400,#14532);
#48=ITEM_DEFINED_TRANSFORMATION($,$,#14389,#14533);
#49=ITEM_DEFINED_TRANSFORMATION($,$,#14400,#14534);
#50=ITEM_DEFINED_TRANSFORMATION($,$,#14389,#14535);
#51=ITEM_DEFINED_TRANSFORMATION($,$,#14400,#14536);
#52=ITEM_DEFINED_TRANSFORMATION($,$,#14428,#14537);
#53=ITEM_DEFINED_TRANSFORMATION($,$,#14473,#14538);
#54=ITEM_DEFINED_TRANSFORMATION($,$,#14473,#14539);
#55=ITEM_DEFINED_TRANSFORMATION($,$,#14473,#14540);
#56=ITEM_DEFINED_TRANSFORMATION($,$,#14499,#14541);
#57=ITEM_DEFINED_TRANSFORMATION($,$,#14499,#14542);
#58=ITEM_DEFINED_TRANSFORMATION($,$,#14499,#14543);
#59=ITEM_DEFINED_TRANSFORMATION($,$,#14499,#14544);
#60=ITEM_DEFINED_TRANSFORMATION($,$,#13561,#14829);
#61=ITEM_DEFINED_TRANSFORMATION($,$,#13616,#14830);
#62=ITEM_DEFINED_TRANSFORMATION($,$,#13663,#14831);
#63=ITEM_DEFINED_TRANSFORMATION($,$,#13694,#14832);
#64=ITEM_DEFINED_TRANSFORMATION($,$,#13716,#14833);
#65=ITEM_DEFINED_TRANSFORMATION($,$,#13747,#14834);
#66=ITEM_DEFINED_TRANSFORMATION($,$,#13770,#14835);
#67=ITEM_DEFINED_TRANSFORMATION($,$,#13799,#14836);
#68=ITEM_DEFINED_TRANSFORMATION($,$,#14499,#14837);
#69=ITEM_DEFINED_TRANSFORMATION($,$,#14499,#14838);
#70=ITEM_DEFINED_TRANSFORMATION($,$,#14499,#14839);
#71=ITEM_DEFINED_TRANSFORMATION($,$,#14499,#14840);
#72=ITEM_DEFINED_TRANSFORMATION($,$,#13828,#14841);
#73=ITEM_DEFINED_TRANSFORMATION($,$,#14473,#14842);
#74=ITEM_DEFINED_TRANSFORMATION($,$,#14473,#14843);
#75=ITEM_DEFINED_TRANSFORMATION($,$,#14473,#14844);
#76=ITEM_DEFINED_TRANSFORMATION($,$,#14473,#14845);
#77=ITEM_DEFINED_TRANSFORMATION($,$,#14499,#14846);
#78=ITEM_DEFINED_TRANSFORMATION($,$,#14499,#14847);
#79=ITEM_DEFINED_TRANSFORMATION($,$,#13871,#14848);
#80=ITEM_DEFINED_TRANSFORMATION($,$,#14473,#14849);
#81=ITEM_DEFINED_TRANSFORMATION($,$,#14473,#14850);
#82=ITEM_DEFINED_TRANSFORMATION($,$,#14473,#14851);
#83=ITEM_DEFINED_TRANSFORMATION($,$,#14803,#14852);
#84=ITEM_DEFINED_TRANSFORMATION($,$,#14803,#14853);
#85=ITEM_DEFINED_TRANSFORMATION($,$,#13999,#14854);
#86=ITEM_DEFINED_TRANSFORMATION($,$,#14473,#14855);
#87=ITEM_DEFINED_TRANSFORMATION($,$,#14473,#14856);
#88=ITEM_DEFINED_TRANSFORMATION($,$,#14473,#14857);
#89=ITEM_DEFINED_TRANSFORMATION($,$,#14499,#14858);
#90=ITEM_DEFINED_TRANSFORMATION($,$,#14499,#14859);
#91=ITEM_DEFINED_TRANSFORMATION($,$,#14499,#14860);
#92=ITEM_DEFINED_TRANSFORMATION($,$,#14499,#14861);
#93=ITEM_DEFINED_TRANSFORMATION($,$,#14133,#14862);
#94=ITEM_DEFINED_TRANSFORMATION($,$,#14183,#14863);
#95=ITEM_DEFINED_TRANSFORMATION($,$,#14200,#14864);
#96=ITEM_DEFINED_TRANSFORMATION($,$,#14211,#14865);
#97=ITEM_DEFINED_TRANSFORMATION($,$,#14183,#14866);
#98=ITEM_DEFINED_TRANSFORMATION($,$,#14200,#14867);
#99=ITEM_DEFINED_TRANSFORMATION($,$,#14211,#14868);
#100=ITEM_DEFINED_TRANSFORMATION($,$,#14133,#14869);
#101=ITEM_DEFINED_TRANSFORMATION($,$,#14183,#14870);
#102=ITEM_DEFINED_TRANSFORMATION($,$,#14200,#14871);
#103=ITEM_DEFINED_TRANSFORMATION($,$,#14211,#14872);
#104=ITEM_DEFINED_TRANSFORMATION($,$,#14183,#14873);
#105=ITEM_DEFINED_TRANSFORMATION($,$,#14200,#14874);
#106=ITEM_DEFINED_TRANSFORMATION($,$,#14211,#14875);
#107=ITEM_DEFINED_TRANSFORMATION($,$,#14546,#14876);
#108=ITEM_DEFINED_TRANSFORMATION($,$,#14701,#14877);
#109=ITEM_DEFINED_TRANSFORMATION($,$,#14710,#14878);
#110=ITEM_DEFINED_TRANSFORMATION($,$,#14724,#14879);
#111=ITEM_DEFINED_TRANSFORMATION($,$,#14748,#14880);
#112=ITEM_DEFINED_TRANSFORMATION($,$,#14757,#14881);
#113=ITEM_DEFINED_TRANSFORMATION($,$,#14766,#14882);
#114=ITEM_DEFINED_TRANSFORMATION($,$,#14777,#14883);
#115=ITEM_DEFINED_TRANSFORMATION($,$,#14777,#14884);
#116=ITEM_DEFINED_TRANSFORMATION($,$,#14794,#14885);
#117=ITEM_DEFINED_TRANSFORMATION($,$,#14803,#14886);
#118=ITEM_DEFINED_TRANSFORMATION($,$,#13560,#14887);
#119=ITEM_DEFINED_TRANSFORMATION($,$,#14235,#14888);
#120=ITEM_DEFINED_TRANSFORMATION($,$,#14545,#14889);
#121=(
REPRESENTATION_RELATIONSHIP($,$,#34194,#34193)
REPRESENTATION_RELATIONSHIP_WITH_TRANSFORMATION(#27)
SHAPE_REPRESENTATION_RELATIONSHIP()
);
#122=(
REPRESENTATION_RELATIONSHIP($,$,#34195,#34193)
REPRESENTATION_RELATIONSHIP_WITH_TRANSFORMATION(#28)
SHAPE_REPRESENTATION_RELATIONSHIP()
);
#123=(
REPRESENTATION_RELATIONSHIP($,$,#34196,#34193)
REPRESENTATION_RELATIONSHIP_WITH_TRANSFORMATION(#29)
SHAPE_REPRESENTATION_RELATIONSHIP()
);
#124=(
REPRESENTATION_RELATIONSHIP($,$,#34197,#34193)
REPRESENTATION_RELATIONSHIP_WITH_TRANSFORMATION(#30)
SHAPE_REPRESENTATION_RELATIONSHIP()
);
#125=(
REPRESENTATION_RELATIONSHIP($,$,#34198,#34193)
REPRESENTATION_RELATIONSHIP_WITH_TRANSFORMATION(#31)
SHAPE_REPRESENTATION_RELATIONSHIP()
);
#126=(
REPRESENTATION_RELATIONSHIP($,$,#34200,#34199)
REPRESENTATION_RELATIONSHIP_WITH_TRANSFORMATION(#32)
SHAPE_REPRESENTATION_RELATIONSHIP()
);
#127=(
REPRESENTATION_RELATIONSHIP($,$,#34201,#34199)
REPRESENTATION_RELATIONSHIP_WITH_TRANSFORMATION(#33)
SHAPE_REPRESENTATION_RELATIONSHIP()
);
#128=(
REPRESENTATION_RELATIONSHIP($,$,#34202,#34199)
REPRESENTATION_RELATIONSHIP_WITH_TRANSFORMATION(#34)
SHAPE_REPRESENTATION_RELATIONSHIP()
);
#129=(
REPRESENTATION_RELATIONSHIP($,$,#34203,#34199)
REPRESENTATION_RELATIONSHIP_WITH_TRANSFORMATION(#35)
SHAPE_REPRESENTATION_RELATIONSHIP()
);
#130=(
REPRESENTATION_RELATIONSHIP($,$,#34204,#34199)
REPRESENTATION_RELATIONSHIP_WITH_TRANSFORMATION(#36)
SHAPE_REPRESENTATION_RELATIONSHIP()
);
#131=(
REPRESENTATION_RELATIONSHIP($,$,#34214,#34213)
REPRESENTATION_RELATIONSHIP_WITH_TRANSFORMATION(#37)
SHAPE_REPRESENTATION_RELATIONSHIP()
);
#132=(
REPRESENTATION_RELATIONSHIP($,$,#34215,#34213)
REPRESENTATION_RELATIONSHIP_WITH_TRANSFORMATION(#38)
SHAPE_REPRESENTATION_RELATIONSHIP()
);
#133=(
REPRESENTATION_RELATIONSHIP($,$,#34216,#34213)
REPRESENTATION_RELATIONSHIP_WITH_TRANSFORMATION(#39)
SHAPE_REPRESENTATION_RELATIONSHIP()
);
#134=(
REPRESENTATION_RELATIONSHIP($,$,#34210,#34209)
REPRESENTATION_RELATIONSHIP_WITH_TRANSFORMATION(#40)
SHAPE_REPRESENTATION_RELATIONSHIP()
);
#135=(
REPRESENTATION_RELATIONSHIP($,$,#34211,#34209)
REPRESENTATION_RELATIONSHIP_WITH_TRANSFORMATION(#41)
SHAPE_REPRESENTATION_RELATIONSHIP()
);
#136=(
REPRESENTATION_RELATIONSHIP($,$,#34212,#34209)
REPRESENTATION_RELATIONSHIP_WITH_TRANSFORMATION(#42)
SHAPE_REPRESENTATION_RELATIONSHIP()
);
#137=(
REPRESENTATION_RELATIONSHIP($,$,#34213,#34209)
REPRESENTATION_RELATIONSHIP_WITH_TRANSFORMATION(#43)
SHAPE_REPRESENTATION_RELATIONSHIP()
);
#138=(
REPRESENTATION_RELATIONSHIP($,$,#34217,#34209)
REPRESENTATION_RELATIONSHIP_WITH_TRANSFORMATION(#44)
SHAPE_REPRESENTATION_RELATIONSHIP()
);
#139=(
REPRESENTATION_RELATIONSHIP($,$,#34218,#34209)
REPRESENTATION_RELATIONSHIP_WITH_TRANSFORMATION(#45)
SHAPE_REPRESENTATION_RELATIONSHIP()
);
#140=(
REPRESENTATION_RELATIONSHIP($,$,#34217,#34209)
REPRESENTATION_RELATIONSHIP_WITH_TRANSFORMATION(#46)
SHAPE_REPRESENTATION_RELATIONSHIP()
);
#141=(
REPRESENTATION_RELATIONSHIP($,$,#34218,#34209)
REPRESENTATION_RELATIONSHIP_WITH_TRANSFORMATION(#47)
SHAPE_REPRESENTATION_RELATIONSHIP()
);
#142=(
REPRESENTATION_RELATIONSHIP($,$,#34217,#34209)
REPRESENTATION_RELATIONSHIP_WITH_TRANSFORMATION(#48)
SHAPE_REPRESENTATION_RELATIONSHIP()
);
#143=(
REPRESENTATION_RELATIONSHIP($,$,#34218,#34209)
REPRESENTATION_RELATIONSHIP_WITH_TRANSFORMATION(#49)
SHAPE_REPRESENTATION_RELATIONSHIP()
);
#144=(
REPRESENTATION_RELATIONSHIP($,$,#34217,#34209)
REPRESENTATION_RELATIONSHIP_WITH_TRANSFORMATION(#50)
SHAPE_REPRESENTATION_RELATIONSHIP()
);
#145=(
REPRESENTATION_RELATIONSHIP($,$,#34218,#34209)
REPRESENTATION_RELATIONSHIP_WITH_TRANSFORMATION(#51)
SHAPE_REPRESENTATION_RELATIONSHIP()
);
#146=(
REPRESENTATION_RELATIONSHIP($,$,#34219,#34209)
REPRESENTATION_RELATIONSHIP_WITH_TRANSFORMATION(#52)
SHAPE_REPRESENTATION_RELATIONSHIP()
);
#147=(
REPRESENTATION_RELATIONSHIP($,$,#34220,#34209)
REPRESENTATION_RELATIONSHIP_WITH_TRANSFORMATION(#53)
SHAPE_REPRESENTATION_RELATIONSHIP()
);
#148=(
REPRESENTATION_RELATIONSHIP($,$,#34220,#34209)
REPRESENTATION_RELATIONSHIP_WITH_TRANSFORMATION(#54)
SHAPE_REPRESENTATION_RELATIONSHIP()
);
#149=(
REPRESENTATION_RELATIONSHIP($,$,#34220,#34209)
REPRESENTATION_RELATIONSHIP_WITH_TRANSFORMATION(#55)
SHAPE_REPRESENTATION_RELATIONSHIP()
);
#150=(
REPRESENTATION_RELATIONSHIP($,$,#34221,#34209)
REPRESENTATION_RELATIONSHIP_WITH_TRANSFORMATION(#56)
SHAPE_REPRESENTATION_RELATIONSHIP()
);
#151=(
REPRESENTATION_RELATIONSHIP($,$,#34221,#34209)
REPRESENTATION_RELATIONSHIP_WITH_TRANSFORMATION(#57)
SHAPE_REPRESENTATION_RELATIONSHIP()
);
#152=(
REPRESENTATION_RELATIONSHIP($,$,#34221,#34209)
REPRESENTATION_RELATIONSHIP_WITH_TRANSFORMATION(#58)
SHAPE_REPRESENTATION_RELATIONSHIP()
);
#153=(
REPRESENTATION_RELATIONSHIP($,$,#34221,#34209)
REPRESENTATION_RELATIONSHIP_WITH_TRANSFORMATION(#59)
SHAPE_REPRESENTATION_RELATIONSHIP()
);
#154=(
REPRESENTATION_RELATIONSHIP($,$,#34184,#34183)
REPRESENTATION_RELATIONSHIP_WITH_TRANSFORMATION(#60)
SHAPE_REPRESENTATION_RELATIONSHIP()
);
#155=(
REPRESENTATION_RELATIONSHIP($,$,#34185,#34183)
REPRESENTATION_RELATIONSHIP_WITH_TRANSFORMATION(#61)
SHAPE_REPRESENTATION_RELATIONSHIP()
);
#156=(
REPRESENTATION_RELATIONSHIP($,$,#34186,#34183)
REPRESENTATION_RELATIONSHIP_WITH_TRANSFORMATION(#62)
SHAPE_REPRESENTATION_RELATIONSHIP()
);
#157=(
REPRESENTATION_RELATIONSHIP($,$,#34187,#34183)
REPRESENTATION_RELATIONSHIP_WITH_TRANSFORMATION(#63)
SHAPE_REPRESENTATION_RELATIONSHIP()
);
#158=(
REPRESENTATION_RELATIONSHIP($,$,#34188,#34183)
REPRESENTATION_RELATIONSHIP_WITH_TRANSFORMATION(#64)
SHAPE_REPRESENTATION_RELATIONSHIP()
);
#159=(
REPRESENTATION_RELATIONSHIP($,$,#34189,#34183)
REPRESENTATION_RELATIONSHIP_WITH_TRANSFORMATION(#65)
SHAPE_REPRESENTATION_RELATIONSHIP()
);
#160=(
REPRESENTATION_RELATIONSHIP($,$,#34190,#34183)
REPRESENTATION_RELATIONSHIP_WITH_TRANSFORMATION(#66)
SHAPE_REPRESENTATION_RELATIONSHIP()
);
#161=(
REPRESENTATION_RELATIONSHIP($,$,#34191,#34183)
REPRESENTATION_RELATIONSHIP_WITH_TRANSFORMATION(#67)
SHAPE_REPRESENTATION_RELATIONSHIP()
);
#162=(
REPRESENTATION_RELATIONSHIP($,$,#34221,#34183)
REPRESENTATION_RELATIONSHIP_WITH_TRANSFORMATION(#68)
SHAPE_REPRESENTATION_RELATIONSHIP()
);
#163=(
REPRESENTATION_RELATIONSHIP($,$,#34221,#34183)
REPRESENTATION_RELATIONSHIP_WITH_TRANSFORMATION(#69)
SHAPE_REPRESENTATION_RELATIONSHIP()
);
#164=(
REPRESENTATION_RELATIONSHIP($,$,#34221,#34183)
REPRESENTATION_RELATIONSHIP_WITH_TRANSFORMATION(#70)
SHAPE_REPRESENTATION_RELATIONSHIP()
);
#165=(
REPRESENTATION_RELATIONSHIP($,$,#34221,#34183)
REPRESENTATION_RELATIONSHIP_WITH_TRANSFORMATION(#71)
SHAPE_REPRESENTATION_RELATIONSHIP()
);
#166=(
REPRESENTATION_RELATIONSHIP($,$,#34192,#34183)
REPRESENTATION_RELATIONSHIP_WITH_TRANSFORMATION(#72)
SHAPE_REPRESENTATION_RELATIONSHIP()
);
#167=(
REPRESENTATION_RELATIONSHIP($,$,#34220,#34183)
REPRESENTATION_RELATIONSHIP_WITH_TRANSFORMATION(#73)
SHAPE_REPRESENTATION_RELATIONSHIP()
);
#168=(
REPRESENTATION_RELATIONSHIP($,$,#34220,#34183)
REPRESENTATION_RELATIONSHIP_WITH_TRANSFORMATION(#74)
SHAPE_REPRESENTATION_RELATIONSHIP()
);
#169=(
REPRESENTATION_RELATIONSHIP($,$,#34220,#34183)
REPRESENTATION_RELATIONSHIP_WITH_TRANSFORMATION(#75)
SHAPE_REPRESENTATION_RELATIONSHIP()
);
#170=(
REPRESENTATION_RELATIONSHIP($,$,#34220,#34183)
REPRESENTATION_RELATIONSHIP_WITH_TRANSFORMATION(#76)
SHAPE_REPRESENTATION_RELATIONSHIP()
);
#171=(
REPRESENTATION_RELATIONSHIP($,$,#34221,#34183)
REPRESENTATION_RELATIONSHIP_WITH_TRANSFORMATION(#77)
SHAPE_REPRESENTATION_RELATIONSHIP()
);
#172=(
REPRESENTATION_RELATIONSHIP($,$,#34221,#34183)
REPRESENTATION_RELATIONSHIP_WITH_TRANSFORMATION(#78)
SHAPE_REPRESENTATION_RELATIONSHIP()
);
#173=(
REPRESENTATION_RELATIONSHIP($,$,#34193,#34183)
REPRESENTATION_RELATIONSHIP_WITH_TRANSFORMATION(#79)
SHAPE_REPRESENTATION_RELATIONSHIP()
);
#174=(
REPRESENTATION_RELATIONSHIP($,$,#34220,#34183)
REPRESENTATION_RELATIONSHIP_WITH_TRANSFORMATION(#80)
SHAPE_REPRESENTATION_RELATIONSHIP()
);
#175=(
REPRESENTATION_RELATIONSHIP($,$,#34220,#34183)
REPRESENTATION_RELATIONSHIP_WITH_TRANSFORMATION(#81)
SHAPE_REPRESENTATION_RELATIONSHIP()
);
#176=(
REPRESENTATION_RELATIONSHIP($,$,#34220,#34183)
REPRESENTATION_RELATIONSHIP_WITH_TRANSFORMATION(#82)
SHAPE_REPRESENTATION_RELATIONSHIP()
);
#177=(
REPRESENTATION_RELATIONSHIP($,$,#34232,#34183)
REPRESENTATION_RELATIONSHIP_WITH_TRANSFORMATION(#83)
SHAPE_REPRESENTATION_RELATIONSHIP()
);
#178=(
REPRESENTATION_RELATIONSHIP($,$,#34232,#34183)
REPRESENTATION_RELATIONSHIP_WITH_TRANSFORMATION(#84)
SHAPE_REPRESENTATION_RELATIONSHIP()
);
#179=(
REPRESENTATION_RELATIONSHIP($,$,#34199,#34183)
REPRESENTATION_RELATIONSHIP_WITH_TRANSFORMATION(#85)
SHAPE_REPRESENTATION_RELATIONSHIP()
);
#180=(
REPRESENTATION_RELATIONSHIP($,$,#34220,#34183)
REPRESENTATION_RELATIONSHIP_WITH_TRANSFORMATION(#86)
SHAPE_REPRESENTATION_RELATIONSHIP()
);
#181=(
REPRESENTATION_RELATIONSHIP($,$,#34220,#34183)
REPRESENTATION_RELATIONSHIP_WITH_TRANSFORMATION(#87)
SHAPE_REPRESENTATION_RELATIONSHIP()
);
#182=(
REPRESENTATION_RELATIONSHIP($,$,#34220,#34183)
REPRESENTATION_RELATIONSHIP_WITH_TRANSFORMATION(#88)
SHAPE_REPRESENTATION_RELATIONSHIP()
);
#183=(
REPRESENTATION_RELATIONSHIP($,$,#34221,#34183)
REPRESENTATION_RELATIONSHIP_WITH_TRANSFORMATION(#89)
SHAPE_REPRESENTATION_RELATIONSHIP()
);
#184=(
REPRESENTATION_RELATIONSHIP($,$,#34221,#34183)
REPRESENTATION_RELATIONSHIP_WITH_TRANSFORMATION(#90)
SHAPE_REPRESENTATION_RELATIONSHIP()
);
#185=(
REPRESENTATION_RELATIONSHIP($,$,#34221,#34183)
REPRESENTATION_RELATIONSHIP_WITH_TRANSFORMATION(#91)
SHAPE_REPRESENTATION_RELATIONSHIP()
);
#186=(
REPRESENTATION_RELATIONSHIP($,$,#34221,#34183)
REPRESENTATION_RELATIONSHIP_WITH_TRANSFORMATION(#92)
SHAPE_REPRESENTATION_RELATIONSHIP()
);
#187=(
REPRESENTATION_RELATIONSHIP($,$,#34205,#34183)
REPRESENTATION_RELATIONSHIP_WITH_TRANSFORMATION(#93)
SHAPE_REPRESENTATION_RELATIONSHIP()
);
#188=(
REPRESENTATION_RELATIONSHIP($,$,#34206,#34183)
REPRESENTATION_RELATIONSHIP_WITH_TRANSFORMATION(#94)
SHAPE_REPRESENTATION_RELATIONSHIP()
);
#189=(
REPRESENTATION_RELATIONSHIP($,$,#34207,#34183)
REPRESENTATION_RELATIONSHIP_WITH_TRANSFORMATION(#95)
SHAPE_REPRESENTATION_RELATIONSHIP()
);
#190=(
REPRESENTATION_RELATIONSHIP($,$,#34208,#34183)
REPRESENTATION_RELATIONSHIP_WITH_TRANSFORMATION(#96)
SHAPE_REPRESENTATION_RELATIONSHIP()
);
#191=(
REPRESENTATION_RELATIONSHIP($,$,#34206,#34183)
REPRESENTATION_RELATIONSHIP_WITH_TRANSFORMATION(#97)
SHAPE_REPRESENTATION_RELATIONSHIP()
);
#192=(
REPRESENTATION_RELATIONSHIP($,$,#34207,#34183)
REPRESENTATION_RELATIONSHIP_WITH_TRANSFORMATION(#98)
SHAPE_REPRESENTATION_RELATIONSHIP()
);
#193=(
REPRESENTATION_RELATIONSHIP($,$,#34208,#34183)
REPRESENTATION_RELATIONSHIP_WITH_TRANSFORMATION(#99)
SHAPE_REPRESENTATION_RELATIONSHIP()
);
#194=(
REPRESENTATION_RELATIONSHIP($,$,#34205,#34183)
REPRESENTATION_RELATIONSHIP_WITH_TRANSFORMATION(#100)
SHAPE_REPRESENTATION_RELATIONSHIP()
);
#195=(
REPRESENTATION_RELATIONSHIP($,$,#34206,#34183)
REPRESENTATION_RELATIONSHIP_WITH_TRANSFORMATION(#101)
SHAPE_REPRESENTATION_RELATIONSHIP()
);
#196=(
REPRESENTATION_RELATIONSHIP($,$,#34207,#34183)
REPRESENTATION_RELATIONSHIP_WITH_TRANSFORMATION(#102)
SHAPE_REPRESENTATION_RELATIONSHIP()
);
#197=(
REPRESENTATION_RELATIONSHIP($,$,#34208,#34183)
REPRESENTATION_RELATIONSHIP_WITH_TRANSFORMATION(#103)
SHAPE_REPRESENTATION_RELATIONSHIP()
);
#198=(
REPRESENTATION_RELATIONSHIP($,$,#34206,#34183)
REPRESENTATION_RELATIONSHIP_WITH_TRANSFORMATION(#104)
SHAPE_REPRESENTATION_RELATIONSHIP()
);
#199=(
REPRESENTATION_RELATIONSHIP($,$,#34207,#34183)
REPRESENTATION_RELATIONSHIP_WITH_TRANSFORMATION(#105)
SHAPE_REPRESENTATION_RELATIONSHIP()
);
#200=(
REPRESENTATION_RELATIONSHIP($,$,#34208,#34183)
REPRESENTATION_RELATIONSHIP_WITH_TRANSFORMATION(#106)
SHAPE_REPRESENTATION_RELATIONSHIP()
);
#201=(
REPRESENTATION_RELATIONSHIP($,$,#34223,#34222)
REPRESENTATION_RELATIONSHIP_WITH_TRANSFORMATION(#107)
SHAPE_REPRESENTATION_RELATIONSHIP()
);
#202=(
REPRESENTATION_RELATIONSHIP($,$,#34224,#34222)
REPRESENTATION_RELATIONSHIP_WITH_TRANSFORMATION(#108)
SHAPE_REPRESENTATION_RELATIONSHIP()
);
#203=(
REPRESENTATION_RELATIONSHIP($,$,#34225,#34222)
REPRESENTATION_RELATIONSHIP_WITH_TRANSFORMATION(#109)
SHAPE_REPRESENTATION_RELATIONSHIP()
);
#204=(
REPRESENTATION_RELATIONSHIP($,$,#34226,#34222)
REPRESENTATION_RELATIONSHIP_WITH_TRANSFORMATION(#110)
SHAPE_REPRESENTATION_RELATIONSHIP()
);
#205=(
REPRESENTATION_RELATIONSHIP($,$,#34227,#34222)
REPRESENTATION_RELATIONSHIP_WITH_TRANSFORMATION(#111)
SHAPE_REPRESENTATION_RELATIONSHIP()
);
#206=(
REPRESENTATION_RELATIONSHIP($,$,#34228,#34222)
REPRESENTATION_RELATIONSHIP_WITH_TRANSFORMATION(#112)
SHAPE_REPRESENTATION_RELATIONSHIP()
);
#207=(
REPRESENTATION_RELATIONSHIP($,$,#34229,#34222)
REPRESENTATION_RELATIONSHIP_WITH_TRANSFORMATION(#113)
SHAPE_REPRESENTATION_RELATIONSHIP()
);
#208=(
REPRESENTATION_RELATIONSHIP($,$,#34230,#34222)
REPRESENTATION_RELATIONSHIP_WITH_TRANSFORMATION(#114)
SHAPE_REPRESENTATION_RELATIONSHIP()
);
#209=(
REPRESENTATION_RELATIONSHIP($,$,#34230,#34222)
REPRESENTATION_RELATIONSHIP_WITH_TRANSFORMATION(#115)
SHAPE_REPRESENTATION_RELATIONSHIP()
);
#210=(
REPRESENTATION_RELATIONSHIP($,$,#34231,#34222)
REPRESENTATION_RELATIONSHIP_WITH_TRANSFORMATION(#116)
SHAPE_REPRESENTATION_RELATIONSHIP()
);
#211=(
REPRESENTATION_RELATIONSHIP($,$,#34232,#34222)
REPRESENTATION_RELATIONSHIP_WITH_TRANSFORMATION(#117)
SHAPE_REPRESENTATION_RELATIONSHIP()
);
#212=(
REPRESENTATION_RELATIONSHIP($,$,#34183,#34182)
REPRESENTATION_RELATIONSHIP_WITH_TRANSFORMATION(#118)
SHAPE_REPRESENTATION_RELATIONSHIP()
);
#213=(
REPRESENTATION_RELATIONSHIP($,$,#34209,#34182)
REPRESENTATION_RELATIONSHIP_WITH_TRANSFORMATION(#119)
SHAPE_REPRESENTATION_RELATIONSHIP()
);
#214=(
REPRESENTATION_RELATIONSHIP($,$,#34222,#34182)
REPRESENTATION_RELATIONSHIP_WITH_TRANSFORMATION(#120)
SHAPE_REPRESENTATION_RELATIONSHIP()
);
#215=CONTEXT_DEPENDENT_SHAPE_REPRESENTATION(#121,#34054);
#216=CONTEXT_DEPENDENT_SHAPE_REPRESENTATION(#122,#34055);
#217=CONTEXT_DEPENDENT_SHAPE_REPRESENTATION(#123,#34056);
#218=CONTEXT_DEPENDENT_SHAPE_REPRESENTATION(#124,#34057);
#219=CONTEXT_DEPENDENT_SHAPE_REPRESENTATION(#125,#34058);
#220=CONTEXT_DEPENDENT_SHAPE_REPRESENTATION(#126,#34065);
#221=CONTEXT_DEPENDENT_SHAPE_REPRESENTATION(#127,#34066);
#222=CONTEXT_DEPENDENT_SHAPE_REPRESENTATION(#128,#34067);
#223=CONTEXT_DEPENDENT_SHAPE_REPRESENTATION(#129,#34068);
#224=CONTEXT_DEPENDENT_SHAPE_REPRESENTATION(#130,#34069);
#225=CONTEXT_DEPENDENT_SHAPE_REPRESENTATION(#131,#34082);
#226=CONTEXT_DEPENDENT_SHAPE_REPRESENTATION(#132,#34083);
#227=CONTEXT_DEPENDENT_SHAPE_REPRESENTATION(#133,#34084);
#228=CONTEXT_DEPENDENT_SHAPE_REPRESENTATION(#134,#34090);
#229=CONTEXT_DEPENDENT_SHAPE_REPRESENTATION(#135,#34091);
#230=CONTEXT_DEPENDENT_SHAPE_REPRESENTATION(#136,#34092);
#231=CONTEXT_DEPENDENT_SHAPE_REPRESENTATION(#137,#34093);
#232=CONTEXT_DEPENDENT_SHAPE_REPRESENTATION(#138,#34094);
#233=CONTEXT_DEPENDENT_SHAPE_REPRESENTATION(#139,#34095);
#234=CONTEXT_DEPENDENT_SHAPE_REPRESENTATION(#140,#34096);
#235=CONTEXT_DEPENDENT_SHAPE_REPRESENTATION(#141,#34097);
#236=CONTEXT_DEPENDENT_SHAPE_REPRESENTATION(#142,#34098);
#237=CONTEXT_DEPENDENT_SHAPE_REPRESENTATION(#143,#34099);
#238=CONTEXT_DEPENDENT_SHAPE_REPRESENTATION(#144,#34100);
#239=CONTEXT_DEPENDENT_SHAPE_REPRESENTATION(#145,#34101);
#240=CONTEXT_DEPENDENT_SHAPE_REPRESENTATION(#146,#34102);
#241=CONTEXT_DEPENDENT_SHAPE_REPRESENTATION(#147,#34103);
#242=CONTEXT_DEPENDENT_SHAPE_REPRESENTATION(#148,#34104);
#243=CONTEXT_DEPENDENT_SHAPE_REPRESENTATION(#149,#34105);
#244=CONTEXT_DEPENDENT_SHAPE_REPRESENTATION(#150,#34106);
#245=CONTEXT_DEPENDENT_SHAPE_REPRESENTATION(#151,#34107);
#246=CONTEXT_DEPENDENT_SHAPE_REPRESENTATION(#152,#34108);
#247=CONTEXT_DEPENDENT_SHAPE_REPRESENTATION(#153,#34109);
#248=CONTEXT_DEPENDENT_SHAPE_REPRESENTATION(#154,#34121);
#249=CONTEXT_DEPENDENT_SHAPE_REPRESENTATION(#155,#34122);
#250=CONTEXT_DEPENDENT_SHAPE_REPRESENTATION(#156,#34123);
#251=CONTEXT_DEPENDENT_SHAPE_REPRESENTATION(#157,#34124);
#252=CONTEXT_DEPENDENT_SHAPE_REPRESENTATION(#158,#34125);
#253=CONTEXT_DEPENDENT_SHAPE_REPRESENTATION(#159,#34126);
#254=CONTEXT_DEPENDENT_SHAPE_REPRESENTATION(#160,#34127);
#255=CONTEXT_DEPENDENT_SHAPE_REPRESENTATION(#161,#34128);
#256=CONTEXT_DEPENDENT_SHAPE_REPRESENTATION(#162,#34129);
#257=CONTEXT_DEPENDENT_SHAPE_REPRESENTATION(#163,#34130);
#258=CONTEXT_DEPENDENT_SHAPE_REPRESENTATION(#164,#34131);
#259=CONTEXT_DEPENDENT_SHAPE_REPRESENTATION(#165,#34132);
#260=CONTEXT_DEPENDENT_SHAPE_REPRESENTATION(#166,#34133);
#261=CONTEXT_DEPENDENT_SHAPE_REPRESENTATION(#167,#34134);
#262=CONTEXT_DEPENDENT_SHAPE_REPRESENTATION(#168,#34135);
#263=CONTEXT_DEPENDENT_SHAPE_REPRESENTATION(#169,#34136);
#264=CONTEXT_DEPENDENT_SHAPE_REPRESENTATION(#170,#34137);
#265=CONTEXT_DEPENDENT_SHAPE_REPRESENTATION(#171,#34138);
#266=CONTEXT_DEPENDENT_SHAPE_REPRESENTATION(#172,#34139);
#267=CONTEXT_DEPENDENT_SHAPE_REPRESENTATION(#173,#34140);
#268=CONTEXT_DEPENDENT_SHAPE_REPRESENTATION(#174,#34141);
#269=CONTEXT_DEPENDENT_SHAPE_REPRESENTATION(#175,#34142);
#270=CONTEXT_DEPENDENT_SHAPE_REPRESENTATION(#176,#34143);
#271=CONTEXT_DEPENDENT_SHAPE_REPRESENTATION(#177,#34144);
#272=CONTEXT_DEPENDENT_SHAPE_REPRESENTATION(#178,#34145);
#273=CONTEXT_DEPENDENT_SHAPE_REPRESENTATION(#179,#34146);
#274=CONTEXT_DEPENDENT_SHAPE_REPRESENTATION(#180,#34147);
#275=CONTEXT_DEPENDENT_SHAPE_REPRESENTATION(#181,#34148);
#276=CONTEXT_DEPENDENT_SHAPE_REPRESENTATION(#182,#34149);
#277=CONTEXT_DEPENDENT_SHAPE_REPRESENTATION(#183,#34150);
#278=CONTEXT_DEPENDENT_SHAPE_REPRESENTATION(#184,#34151);
#279=CONTEXT_DEPENDENT_SHAPE_REPRESENTATION(#185,#34152);
#280=CONTEXT_DEPENDENT_SHAPE_REPRESENTATION(#186,#34153);
#281=CONTEXT_DEPENDENT_SHAPE_REPRESENTATION(#187,#34154);
#282=CONTEXT_DEPENDENT_SHAPE_REPRESENTATION(#188,#34155);
#283=CONTEXT_DEPENDENT_SHAPE_REPRESENTATION(#189,#34156);
#284=CONTEXT_DEPENDENT_SHAPE_REPRESENTATION(#190,#34157);
#285=CONTEXT_DEPENDENT_SHAPE_REPRESENTATION(#191,#34158);
#286=CONTEXT_DEPENDENT_SHAPE_REPRESENTATION(#192,#34159);
#287=CONTEXT_DEPENDENT_SHAPE_REPRESENTATION(#193,#34160);
#288=CONTEXT_DEPENDENT_SHAPE_REPRESENTATION(#194,#34161);
#289=CONTEXT_DEPENDENT_SHAPE_REPRESENTATION(#195,#34162);
#290=CONTEXT_DEPENDENT_SHAPE_REPRESENTATION(#196,#34163);
#291=CONTEXT_DEPENDENT_SHAPE_REPRESENTATION(#197,#34164);
#292=CONTEXT_DEPENDENT_SHAPE_REPRESENTATION(#198,#34165);
#293=CONTEXT_DEPENDENT_SHAPE_REPRESENTATION(#199,#34166);
#294=CONTEXT_DEPENDENT_SHAPE_REPRESENTATION(#200,#34167);
#295=CONTEXT_DEPENDENT_SHAPE_REPRESENTATION(#201,#34168);
#296=CONTEXT_DEPENDENT_SHAPE_REPRESENTATION(#202,#34169);
#297=CONTEXT_DEPENDENT_SHAPE_REPRESENTATION(#203,#34170);
#298=CONTEXT_DEPENDENT_SHAPE_REPRESENTATION(#204,#34171);
#299=CONTEXT_DEPENDENT_SHAPE_REPRESENTATION(#205,#34172);
#300=CONTEXT_DEPENDENT_SHAPE_REPRESENTATION(#206,#34173);
#301=CONTEXT_DEPENDENT_SHAPE_REPRESENTATION(#207,#34174);
#302=CONTEXT_DEPENDENT_SHAPE_REPRESENTATION(#208,#34175);
#303=CONTEXT_DEPENDENT_SHAPE_REPRESENTATION(#209,#34176);
#304=CONTEXT_DEPENDENT_SHAPE_REPRESENTATION(#210,#34177);
#305=CONTEXT_DEPENDENT_SHAPE_REPRESENTATION(#211,#34178);
#306=CONTEXT_DEPENDENT_SHAPE_REPRESENTATION(#212,#34179);
#307=CONTEXT_DEPENDENT_SHAPE_REPRESENTATION(#213,#34180);
#308=CONTEXT_DEPENDENT_SHAPE_REPRESENTATION(#214,#34181);
#309=NEXT_ASSEMBLY_USAGE_OCCURRENCE('Inner ring:1','Inner ring:1',
'Inner ring:1',#34245,#34246,'Inner ring:1');
#310=NEXT_ASSEMBLY_USAGE_OCCURRENCE('Outer ring:1','Outer ring:1',
'Outer ring:1',#34245,#34247,'Outer ring:1');
#311=NEXT_ASSEMBLY_USAGE_OCCURRENCE('Balls:1','Balls:1','Balls:1',#34245,
#34248,'Balls:1');
#312=NEXT_ASSEMBLY_USAGE_OCCURRENCE('Cage:1','Cage:1','Cage:1',#34245,#34249,
'Cage:1');
#313=NEXT_ASSEMBLY_USAGE_OCCURRENCE('Seals 2RS:1','Seals 2RS:1',
'Seals 2RS:1',#34245,#34250,'Seals 2RS:1');
#314=NEXT_ASSEMBLY_USAGE_OCCURRENCE('Inner ring (1):1',
'Inner ring (1):1','Inner ring (1):1',#34251,#34252,'Inner ring (1):1');
#315=NEXT_ASSEMBLY_USAGE_OCCURRENCE('Outer ring (1):1',
'Outer ring (1):1','Outer ring (1):1',#34251,#34253,'Outer ring (1):1');
#316=NEXT_ASSEMBLY_USAGE_OCCURRENCE('Balls (1):1','Balls (1):1',
'Balls (1):1',#34251,#34254,'Balls (1):1');
#317=NEXT_ASSEMBLY_USAGE_OCCURRENCE('Cage (1):1','Cage (1):1',
'Cage (1):1',#34251,#34255,'Cage (1):1');
#318=NEXT_ASSEMBLY_USAGE_OCCURRENCE('Seals 2RS (1):1','Seals 2RS (1):1',
'Seals 2RS (1):1',#34251,#34256,'Seals 2RS (1):1');
#319=NEXT_ASSEMBLY_USAGE_OCCURRENCE('Block:1','Block:1','Block:1',#34265,
#34266,'Block:1');
#320=NEXT_ASSEMBLY_USAGE_OCCURRENCE('End cap +:1','End cap +:1',
'End cap +:1',#34265,#34267,'End cap +:1');
#321=NEXT_ASSEMBLY_USAGE_OCCURRENCE('End cap:1','End cap:1','End cap:1',
#34265,#34268,'End cap:1');
#322=NEXT_ASSEMBLY_USAGE_OCCURRENCE('Carriage spacer:1',
'Carriage spacer:1','Carriage spacer:1',#34261,#34262,
'Carriage spacer:1');
#323=NEXT_ASSEMBLY_USAGE_OCCURRENCE('Table:1','Table:1','Table:1',#34261,
#34263,'Table:1');
#324=NEXT_ASSEMBLY_USAGE_OCCURRENCE('Nut bracket:1','Nut bracket:1',
'Nut bracket:1',#34261,#34264,'Nut bracket:1');
#325=NEXT_ASSEMBLY_USAGE_OCCURRENCE(
'Flanged Linear Guide Carriage - 15 mm:2',
'Flanged Linear Guide Carriage - 15 mm:2',
'Flanged Linear Guide Carriage - 15 mm:2',#34261,#34265,
'Flanged Linear Guide Carriage - 15 mm:2');
#326=NEXT_ASSEMBLY_USAGE_OCCURRENCE('Flat Washer - M5 (1):2',
'Flat Washer - M5 (1):2','Flat Washer - M5 (1):2',#34261,#34269,
'Flat Washer - M5 (1):2');
#327=NEXT_ASSEMBLY_USAGE_OCCURRENCE('M5x30 frame screw:2',
'M5x30 frame screw:2','M5x30 frame screw:2',#34261,#34270,
'M5x30 frame screw:2');
#328=NEXT_ASSEMBLY_USAGE_OCCURRENCE('Flat Washer - M5 (1):3',
'Flat Washer - M5 (1):3','Flat Washer - M5 (1):3',#34261,#34269,
'Flat Washer - M5 (1):3');
#329=NEXT_ASSEMBLY_USAGE_OCCURRENCE('M5x30 frame screw:3',
'M5x30 frame screw:3','M5x30 frame screw:3',#34261,#34270,
'M5x30 frame screw:3');
#330=NEXT_ASSEMBLY_USAGE_OCCURRENCE('Flat Washer - M5 (1):4',
'Flat Washer - M5 (1):4','Flat Washer - M5 (1):4',#34261,#34269,
'Flat Washer - M5 (1):4');
#331=NEXT_ASSEMBLY_USAGE_OCCURRENCE('M5x30 frame screw:4',
'M5x30 frame screw:4','M5x30 frame screw:4',#34261,#34270,
'M5x30 frame screw:4');
#332=NEXT_ASSEMBLY_USAGE_OCCURRENCE('Flat Washer - M5 (1):5',
'Flat Washer - M5 (1):5','Flat Washer - M5 (1):5',#34261,#34269,
'Flat Washer - M5 (1):5');
#333=NEXT_ASSEMBLY_USAGE_OCCURRENCE('M5x30 frame screw:5',
'M5x30 frame screw:5','M5x30 frame screw:5',#34261,#34270,
'M5x30 frame screw:5');
#334=NEXT_ASSEMBLY_USAGE_OCCURRENCE('Flanged lead nut:2',
'Flanged lead nut:2','Flanged lead nut:2',#34261,#34271,
'Flanged lead nut:2');
#335=NEXT_ASSEMBLY_USAGE_OCCURRENCE('Cap Screw - M4x16:6',
'Cap Screw - M4x16:6','Cap Screw - M4x16:6',#34261,#34272,
'Cap Screw - M4x16:6');
#336=NEXT_ASSEMBLY_USAGE_OCCURRENCE('Cap Screw - M4x16:7',
'Cap Screw - M4x16:7','Cap Screw - M4x16:7',#34261,#34272,
'Cap Screw - M4x16:7');
#337=NEXT_ASSEMBLY_USAGE_OCCURRENCE('Cap Screw - M4x16:8',
'Cap Screw - M4x16:8','Cap Screw - M4x16:8',#34261,#34272,
'Cap Screw - M4x16:8');
#338=NEXT_ASSEMBLY_USAGE_OCCURRENCE('Cap Screw - M5x20:6',
'Cap Screw - M5x20:6','Cap Screw - M5x20:6',#34261,#34273,
'Cap Screw - M5x20:6');
#339=NEXT_ASSEMBLY_USAGE_OCCURRENCE('Cap Screw - M5x20:7',
'Cap Screw - M5x20:7','Cap Screw - M5x20:7',#34261,#34273,
'Cap Screw - M5x20:7');
#340=NEXT_ASSEMBLY_USAGE_OCCURRENCE('Cap Screw - M5x20:8',
'Cap Screw - M5x20:8','Cap Screw - M5x20:8',#34261,#34273,
'Cap Screw - M5x20:8');
#341=NEXT_ASSEMBLY_USAGE_OCCURRENCE('Cap Screw - M5x20:9',
'Cap Screw - M5x20:9','Cap Screw - M5x20:9',#34261,#34273,
'Cap Screw - M5x20:9');
#342=NEXT_ASSEMBLY_USAGE_OCCURRENCE('Runner-mounted base:1',
'Runner-mounted base:1','Runner-mounted base:1',#34235,#34236,
'Runner-mounted base:1');
#343=NEXT_ASSEMBLY_USAGE_OCCURRENCE('Rail adapter:1','Rail adapter:1',
'Rail adapter:1',#34235,#34237,'Rail adapter:1');
#344=NEXT_ASSEMBLY_USAGE_OCCURRENCE('Floating bearing support:1',
'Floating bearing support:1','Floating bearing support:1',#34235,#34238,
'Floating bearing support:1');
#345=NEXT_ASSEMBLY_USAGE_OCCURRENCE('Floating cap:1','Floating cap:1',
'Floating cap:1',#34235,#34239,'Floating cap:1');
#346=NEXT_ASSEMBLY_USAGE_OCCURRENCE('Fixed bearing support:1',
'Fixed bearing support:1','Fixed bearing support:1',#34235,#34240,
'Fixed bearing support:1');
#347=NEXT_ASSEMBLY_USAGE_OCCURRENCE('Fixed cap:1','Fixed cap:1',
'Fixed cap:1',#34235,#34241,'Fixed cap:1');
#348=NEXT_ASSEMBLY_USAGE_OCCURRENCE('End stop:1','End stop:1',
'End stop:1',#34235,#34242,'End stop:1');
#349=NEXT_ASSEMBLY_USAGE_OCCURRENCE('End stop (1):1','End stop (1):1',
'End stop (1):1',#34235,#34243,'End stop (1):1');
#350=NEXT_ASSEMBLY_USAGE_OCCURRENCE('Cap Screw - M5x20:2',
'Cap Screw - M5x20:2','Cap Screw - M5x20:2',#34235,#34273,
'Cap Screw - M5x20:2');
#351=NEXT_ASSEMBLY_USAGE_OCCURRENCE('Cap Screw - M5x20:3',
'Cap Screw - M5x20:3','Cap Screw - M5x20:3',#34235,#34273,
'Cap Screw - M5x20:3');
#352=NEXT_ASSEMBLY_USAGE_OCCURRENCE('Cap Screw - M5x20:4',
'Cap Screw - M5x20:4','Cap Screw - M5x20:4',#34235,#34273,
'Cap Screw - M5x20:4');
#353=NEXT_ASSEMBLY_USAGE_OCCURRENCE('Cap Screw - M5x20:5',
'Cap Screw - M5x20:5','Cap Screw - M5x20:5',#34235,#34273,
'Cap Screw - M5x20:5');
#354=NEXT_ASSEMBLY_USAGE_OCCURRENCE(
'Linear Guide Rail - 15 mm, 220 mm Long:2',
'Linear Guide Rail - 15 mm, 220 mm Long:2',
'Linear Guide Rail - 15 mm, 220 mm Long:2',#34235,#34244,
'Linear Guide Rail - 15 mm, 220 mm Long:2');
#355=NEXT_ASSEMBLY_USAGE_OCCURRENCE('Cap Screw - M4x16:2',
'Cap Screw - M4x16:2','Cap Screw - M4x16:2',#34235,#34272,
'Cap Screw - M4x16:2');
#356=NEXT_ASSEMBLY_USAGE_OCCURRENCE('Cap Screw - M4x16:3',
'Cap Screw - M4x16:3','Cap Screw - M4x16:3',#34235,#34272,
'Cap Screw - M4x16:3');
#357=NEXT_ASSEMBLY_USAGE_OCCURRENCE('Cap Screw - M4x16:4',
'Cap Screw - M4x16:4','Cap Screw - M4x16:4',#34235,#34272,
'Cap Screw - M4x16:4');
#358=NEXT_ASSEMBLY_USAGE_OCCURRENCE('Cap Screw - M4x16:5',
'Cap Screw - M4x16:5','Cap Screw - M4x16:5',#34235,#34272,
'Cap Screw - M4x16:5');
#359=NEXT_ASSEMBLY_USAGE_OCCURRENCE('Cap Screw - M5x20:10',
'Cap Screw - M5x20:10','Cap Screw - M5x20:10',#34235,#34273,
'Cap Screw - M5x20:10');
#360=NEXT_ASSEMBLY_USAGE_OCCURRENCE('Cap Screw - M5x20:11',
'Cap Screw - M5x20:11','Cap Screw - M5x20:11',#34235,#34273,
'Cap Screw - M5x20:11');
#361=NEXT_ASSEMBLY_USAGE_OCCURRENCE(
'Sealed Ball Bearing - 12 x 32 x 10 mm:2',
'Sealed Ball Bearing - 12 x 32 x 10 mm:2',
'Sealed Ball Bearing - 12 x 32 x 10 mm:2',#34235,#34245,
'Sealed Ball Bearing - 12 x 32 x 10 mm:2');
#362=NEXT_ASSEMBLY_USAGE_OCCURRENCE('Cap Screw - M4x16:9',
'Cap Screw - M4x16:9','Cap Screw - M4x16:9',#34235,#34272,
'Cap Screw - M4x16:9');
#363=NEXT_ASSEMBLY_USAGE_OCCURRENCE('Cap Screw - M4x16:10',
'Cap Screw - M4x16:10','Cap Screw - M4x16:10',#34235,#34272,
'Cap Screw - M4x16:10');
#364=NEXT_ASSEMBLY_USAGE_OCCURRENCE('Cap Screw - M4x16:11',
'Cap Screw - M4x16:11','Cap Screw - M4x16:11',#34235,#34272,
'Cap Screw - M4x16:11');
#365=NEXT_ASSEMBLY_USAGE_OCCURRENCE('Cap Screw - M6x25:2',
'Cap Screw - M6x25:2','Cap Screw - M6x25:2',#34235,#34284,
'Cap Screw - M6x25:2');
#366=NEXT_ASSEMBLY_USAGE_OCCURRENCE('Cap Screw - M6x25:3',
'Cap Screw - M6x25:3','Cap Screw - M6x25:3',#34235,#34284,
'Cap Screw - M6x25:3');
#367=NEXT_ASSEMBLY_USAGE_OCCURRENCE(
'Sealed Ball Bearing - 20 x 47 x 14 mm:2',
'Sealed Ball Bearing - 20 x 47 x 14 mm:2',
'Sealed Ball Bearing - 20 x 47 x 14 mm:2',#34235,#34251,
'Sealed Ball Bearing - 20 x 47 x 14 mm:2');
#368=NEXT_ASSEMBLY_USAGE_OCCURRENCE('Cap Screw - M4x16:12',
'Cap Screw - M4x16:12','Cap Screw - M4x16:12',#34235,#34272,
'Cap Screw - M4x16:12');
#369=NEXT_ASSEMBLY_USAGE_OCCURRENCE('Cap Screw - M4x16:13',
'Cap Screw - M4x16:13','Cap Screw - M4x16:13',#34235,#34272,
'Cap Screw - M4x16:13');
#370=NEXT_ASSEMBLY_USAGE_OCCURRENCE('Cap Screw - M4x16:14',
'Cap Screw - M4x16:14','Cap Screw - M4x16:14',#34235,#34272,
'Cap Screw - M4x16:14');
#371=NEXT_ASSEMBLY_USAGE_OCCURRENCE('Cap Screw - M5x20:12',
'Cap Screw - M5x20:12','Cap Screw - M5x20:12',#34235,#34273,
'Cap Screw - M5x20:12');
#372=NEXT_ASSEMBLY_USAGE_OCCURRENCE('Cap Screw - M5x20:13',
'Cap Screw - M5x20:13','Cap Screw - M5x20:13',#34235,#34273,
'Cap Screw - M5x20:13');
#373=NEXT_ASSEMBLY_USAGE_OCCURRENCE('Cap Screw - M5x20:14',
'Cap Screw - M5x20:14','Cap Screw - M5x20:14',#34235,#34273,
'Cap Screw - M5x20:14');
#374=NEXT_ASSEMBLY_USAGE_OCCURRENCE('Cap Screw - M5x20:15',
'Cap Screw - M5x20:15','Cap Screw - M5x20:15',#34235,#34273,
'Cap Screw - M5x20:15');
#375=NEXT_ASSEMBLY_USAGE_OCCURRENCE(
'Slotted Extrusion - 20 x 20 x 300 mm:2',
'Slotted Extrusion - 20 x 20 x 300 mm:2',
'Slotted Extrusion - 20 x 20 x 300 mm:2',#34235,#34257,
'Slotted Extrusion - 20 x 20 x 300 mm:2');
#376=NEXT_ASSEMBLY_USAGE_OCCURRENCE(
'Slot Nut - M5 for 20 mm Extrusion:2',
'Slot Nut - M5 for 20 mm Extrusion:2',
'Slot Nut - M5 for 20 mm Extrusion:2',#34235,#34258,
'Slot Nut - M5 for 20 mm Extrusion:2');
#377=NEXT_ASSEMBLY_USAGE_OCCURRENCE('Flat Washer - M5:2',
'Flat Washer - M5:2','Flat Washer - M5:2',#34235,#34259,
'Flat Washer - M5:2');
#378=NEXT_ASSEMBLY_USAGE_OCCURRENCE('M5x18 runner screw:2',
'M5x18 runner screw:2','M5x18 runner screw:2',#34235,#34260,
'M5x18 runner screw:2');
#379=NEXT_ASSEMBLY_USAGE_OCCURRENCE(
'Slot Nut - M5 for 20 mm Extrusion:3',
'Slot Nut - M5 for 20 mm Extrusion:3',
'Slot Nut - M5 for 20 mm Extrusion:3',#34235,#34258,
'Slot Nut - M5 for 20 mm Extrusion:3');
#380=NEXT_ASSEMBLY_USAGE_OCCURRENCE('Flat Washer - M5:3',
'Flat Washer - M5:3','Flat Washer - M5:3',#34235,#34259,
'Flat Washer - M5:3');
#381=NEXT_ASSEMBLY_USAGE_OCCURRENCE('M5x18 runner screw:3',
'M5x18 runner screw:3','M5x18 runner screw:3',#34235,#34260,
'M5x18 runner screw:3');
#382=NEXT_ASSEMBLY_USAGE_OCCURRENCE(
'Slotted Extrusion - 20 x 20 x 300 mm:3',
'Slotted Extrusion - 20 x 20 x 300 mm:3',
'Slotted Extrusion - 20 x 20 x 300 mm:3',#34235,#34257,
'Slotted Extrusion - 20 x 20 x 300 mm:3');
#383=NEXT_ASSEMBLY_USAGE_OCCURRENCE(
'Slot Nut - M5 for 20 mm Extrusion:4',
'Slot Nut - M5 for 20 mm Extrusion:4',
'Slot Nut - M5 for 20 mm Extrusion:4',#34235,#34258,
'Slot Nut - M5 for 20 mm Extrusion:4');
#384=NEXT_ASSEMBLY_USAGE_OCCURRENCE('Flat Washer - M5:4',
'Flat Washer - M5:4','Flat Washer - M5:4',#34235,#34259,
'Flat Washer - M5:4');
#385=NEXT_ASSEMBLY_USAGE_OCCURRENCE('M5x18 runner screw:4',
'M5x18 runner screw:4','M5x18 runner screw:4',#34235,#34260,
'M5x18 runner screw:4');
#386=NEXT_ASSEMBLY_USAGE_OCCURRENCE(
'Slot Nut - M5 for 20 mm Extrusion:5',
'Slot Nut - M5 for 20 mm Extrusion:5',
'Slot Nut - M5 for 20 mm Extrusion:5',#34235,#34258,
'Slot Nut - M5 for 20 mm Extrusion:5');
#387=NEXT_ASSEMBLY_USAGE_OCCURRENCE('Flat Washer - M5:5',
'Flat Washer - M5:5','Flat Washer - M5:5',#34235,#34259,
'Flat Washer - M5:5');
#388=NEXT_ASSEMBLY_USAGE_OCCURRENCE('M5x18 runner screw:5',
'M5x18 runner screw:5','M5x18 runner screw:5',#34235,#34260,
'M5x18 runner screw:5');
#389=NEXT_ASSEMBLY_USAGE_OCCURRENCE('Supported TR12x3 screw:2',
'Supported TR12x3 screw:2','Supported TR12x3 screw:2',#34274,#34275,
'Supported TR12x3 screw:2');
#390=NEXT_ASSEMBLY_USAGE_OCCURRENCE('Inner race spacer:2',
'Inner race spacer:2','Inner race spacer:2',#34274,#34276,
'Inner race spacer:2');
#391=NEXT_ASSEMBLY_USAGE_OCCURRENCE('Shaft retaining collar:2',
'Shaft retaining collar:2','Shaft retaining collar:2',#34274,#34277,
'Shaft retaining collar:2');
#392=NEXT_ASSEMBLY_USAGE_OCCURRENCE('Handwheel:2','Handwheel:2',
'Handwheel:2',#34274,#34278,'Handwheel:2');
#393=NEXT_ASSEMBLY_USAGE_OCCURRENCE('Handle pivot sleeve:2',
'Handle pivot sleeve:2','Handle pivot sleeve:2',#34274,#34279,
'Handle pivot sleeve:2');
#394=NEXT_ASSEMBLY_USAGE_OCCURRENCE('Revolving handle:2',
'Revolving handle:2','Revolving handle:2',#34274,#34280,
'Revolving handle:2');
#395=NEXT_ASSEMBLY_USAGE_OCCURRENCE('Key 6x6x20:2','Key 6x6x20:2',
'Key 6x6x20:2',#34274,#34281,'Key 6x6x20:2');
#396=NEXT_ASSEMBLY_USAGE_OCCURRENCE('Socket Set Screw - M5x8:2',
'Socket Set Screw - M5x8:2','Socket Set Screw - M5x8:2',#34274,#34282,
'Socket Set Screw - M5x8:2');
#397=NEXT_ASSEMBLY_USAGE_OCCURRENCE('Socket Set Screw - M5x8:3',
'Socket Set Screw - M5x8:3','Socket Set Screw - M5x8:3',#34274,#34282,
'Socket Set Screw - M5x8:3');
#398=NEXT_ASSEMBLY_USAGE_OCCURRENCE('Flat Washer - M6:2',
'Flat Washer - M6:2','Flat Washer - M6:2',#34274,#34283,
'Flat Washer - M6:2');
#399=NEXT_ASSEMBLY_USAGE_OCCURRENCE('Cap Screw - M6x25:4',
'Cap Screw - M6x25:4','Cap Screw - M6x25:4',#34274,#34284,
'Cap Screw - M6x25:4');
#400=NEXT_ASSEMBLY_USAGE_OCCURRENCE('Rail and screw supports:1',
'Rail and screw supports:1','Rail and screw supports:1',#34234,#34235,
'Rail and screw supports:1');
#401=NEXT_ASSEMBLY_USAGE_OCCURRENCE('Moving table and nut:1',
'Moving table and nut:1','Moving table and nut:1',#34234,#34261,
'Moving table and nut:1');
#402=NEXT_ASSEMBLY_USAGE_OCCURRENCE('Lead screw and handwheel:1',
'Lead screw and handwheel:1','Lead screw and handwheel:1',#34234,#34274,
'Lead screw and handwheel:1');
#403=B_SPLINE_CURVE_WITH_KNOTS('',3,(#19369,#19370,#19371,#19372,#19373,
#19374,#19375,#19376,#19377,#19378,#19379,#19380,#19381,#19382,#19383,#19384,
#19385,#19386,#19387,#19388,#19389,#19390),.UNSPECIFIED.,.F.,.F.,(4,2,2,
2,2,2,2,2,2,2,4),(0.0591825211272536,0.157966726598481,0.236950089897721,
0.315933453196962,0.391576304923761,0.46721915665056,0.54286200837736,0.618504860104159,
0.697488223403399,0.77647158670264,0.875255792173867),.UNSPECIFIED.);
#404=B_SPLINE_CURVE_WITH_KNOTS('',3,(#19394,#19395,#19396,#19397,#19398,
#19399,#19400,#19401,#19402,#19403,#19404,#19405,#19406,#19407,#19408,#19409,
#19410,#19411,#19412,#19413,#19414,#19415),.UNSPECIFIED.,.F.,.F.,(4,2,2,
2,2,2,2,2,2,2,4),(0.0581119756758434,0.106553146291161,0.213106292582322,
0.30849933801665,0.386091982889075,0.4636846277615,0.541277272633925,0.61886991750635,
0.714262962940678,0.820816109231839,0.869257279847157),.UNSPECIFIED.);
#405=B_SPLINE_CURVE_WITH_KNOTS('',3,(#19421,#19422,#19423,#19424,#19425,
#19426,#19427,#19428,#19429,#19430,#19431,#19432,#19433,#19434,#19435,#19436,
#19437,#19438,#19439,#19440,#19441,#19442),.UNSPECIFIED.,.F.,.F.,(4,2,2,
2,2,2,2,2,2,2,4),(0.0581119756758434,0.106553146291161,0.213106292582322,
0.30849933801665,0.386091982889075,0.4636846277615,0.541277272633925,0.61886991750635,
0.714262962940679,0.820816109231839,0.869257279847157),.UNSPECIFIED.);
#406=B_SPLINE_CURVE_WITH_KNOTS('',3,(#19446,#19447,#19448,#19449,#19450,
#19451,#19452,#19453,#19454,#19455,#19456,#19457,#19458,#19459,#19460,#19461,
#19462,#19463,#19464,#19465,#19466,#19467),.UNSPECIFIED.,.F.,.F.,(4,2,2,
2,2,2,2,2,2,2,4),(0.0581119756758433,0.106553146291161,0.213106292582322,
0.308499338016649,0.386091982889075,0.4636846277615,0.541277272633925,0.61886991750635,
0.714262962940678,0.820816109231839,0.869257279847157),.UNSPECIFIED.);
#407=B_SPLINE_CURVE_WITH_KNOTS('',3,(#19476,#19477,#19478,#19479,#19480,
#19481,#19482,#19483,#19484,#19485,#19486,#19487,#19488,#19489,#19490,#19491,
#19492,#19493,#19494,#19495,#19496,#19497),.UNSPECIFIED.,.F.,.F.,(4,2,2,
2,2,2,2,2,2,2,4),(0.0581119756758433,0.106553146291161,0.213106292582322,
0.30849933801665,0.386091982889075,0.4636846277615,0.541277272633925,0.61886991750635,
0.714262962940678,0.820816109231839,0.869257279847157),.UNSPECIFIED.);
#408=B_SPLINE_CURVE_WITH_KNOTS('',3,(#19501,#19502,#19503,#19504,#19505,
#19506,#19507,#19508,#19509,#19510,#19511,#19512,#19513,#19514,#19515,#19516,
#19517,#19518,#19519,#19520,#19521,#19522),.UNSPECIFIED.,.F.,.F.,(4,2,2,
2,2,2,2,2,2,2,4),(0.0581119756758434,0.106553146291161,0.213106292582322,
0.30849933801665,0.386091982889075,0.4636846277615,0.541277272633925,0.61886991750635,
0.714262962940678,0.820816109231839,0.869257279847157),.UNSPECIFIED.);
#409=B_SPLINE_CURVE_WITH_KNOTS('',3,(#19526,#19527,#19528,#19529,#19530,
#19531,#19532,#19533,#19534,#19535,#19536,#19537,#19538,#19539,#19540,#19541,
#19542,#19543,#19544,#19545,#19546,#19547),.UNSPECIFIED.,.F.,.F.,(4,2,2,
2,2,2,2,2,2,2,4),(0.0581119756758434,0.106553146291161,0.213106292582322,
0.30849933801665,0.386091982889075,0.4636846277615,0.541277272633925,0.61886991750635,
0.714262962940678,0.820816109231839,0.869257279847157),.UNSPECIFIED.);
#410=B_SPLINE_CURVE_WITH_KNOTS('',3,(#19551,#19552,#19553,#19554,#19555,
#19556,#19557,#19558,#19559,#19560,#19561,#19562,#19563,#19564,#19565,#19566,
#19567,#19568,#19569,#19570,#19571,#19572),.UNSPECIFIED.,.F.,.F.,(4,2,2,
2,2,2,2,2,2,2,4),(0.0581119756758433,0.106553146291161,0.213106292582322,
0.30849933801665,0.386091982889075,0.4636846277615,0.541277272633925,0.61886991750635,
0.714262962940678,0.820816109231839,0.869257279847157),.UNSPECIFIED.);
#411=B_SPLINE_CURVE_WITH_KNOTS('',3,(#19580,#19581,#19582,#19583,#19584,
#19585,#19586,#19587,#19588,#19589,#19590,#19591,#19592,#19593,#19594,#19595,
#19596,#19597,#19598,#19599,#19600,#19601),.UNSPECIFIED.,.F.,.F.,(4,2,2,
2,2,2,2,2,2,2,4),(0.0591825211272536,0.157966726598481,0.236950089897721,
0.315933453196962,0.391576304923761,0.467219156650561,0.54286200837736,
0.618504860104159,0.697488223403399,0.77647158670264,0.875255792173867),
 .UNSPECIFIED.);
#412=B_SPLINE_CURVE_WITH_KNOTS('',3,(#19609,#19610,#19611,#19612,#19613,
#19614,#19615,#19616,#19617,#19618,#19619,#19620,#19621,#19622,#19623,#19624,
#19625,#19626,#19627,#19628,#19629,#19630),.UNSPECIFIED.,.F.,.F.,(4,2,2,
2,2,2,2,2,2,2,4),(0.0591825211272536,0.157966726598481,0.236950089897722,
0.315933453196962,0.391576304923761,0.467219156650561,0.54286200837736,
0.618504860104159,0.697488223403399,0.77647158670264,0.875255792173867),
 .UNSPECIFIED.);
#413=B_SPLINE_CURVE_WITH_KNOTS('',3,(#19640,#19641,#19642,#19643,#19644,
#19645,#19646,#19647,#19648,#19649,#19650,#19651,#19652,#19653,#19654,#19655,
#19656,#19657,#19658,#19659,#19660,#19661),.UNSPECIFIED.,.F.,.F.,(4,2,2,
2,2,2,2,2,2,2,4),(0.0591825211272536,0.157966726598481,0.236950089897721,
0.315933453196962,0.391576304923761,0.46721915665056,0.54286200837736,0.618504860104159,
0.697488223403399,0.77647158670264,0.875255792173867),.UNSPECIFIED.);
#414=B_SPLINE_CURVE_WITH_KNOTS('',3,(#19669,#19670,#19671,#19672,#19673,
#19674,#19675,#19676,#19677,#19678,#19679,#19680,#19681,#19682,#19683,#19684,
#19685,#19686,#19687,#19688,#19689,#19690),.UNSPECIFIED.,.F.,.F.,(4,2,2,
2,2,2,2,2,2,2,4),(0.0591825211272536,0.157966726598481,0.236950089897721,
0.315933453196962,0.391576304923761,0.46721915665056,0.542862008377359,
0.618504860104159,0.697488223403399,0.776471586702639,0.875255792173867),
 .UNSPECIFIED.);
#415=B_SPLINE_CURVE_WITH_KNOTS('',3,(#19698,#19699,#19700,#19701,#19702,
#19703,#19704,#19705,#19706,#19707,#19708,#19709,#19710,#19711,#19712,#19713,
#19714,#19715,#19716,#19717,#19718,#19719),.UNSPECIFIED.,.F.,.F.,(4,2,2,
2,2,2,2,2,2,2,4),(0.0591825211272536,0.157966726598481,0.236950089897721,
0.315933453196962,0.391576304923761,0.46721915665056,0.54286200837736,0.618504860104159,
0.697488223403399,0.77647158670264,0.875255792173867),.UNSPECIFIED.);
#416=B_SPLINE_CURVE_WITH_KNOTS('',3,(#19728,#19729,#19730,#19731,#19732,
#19733,#19734,#19735,#19736,#19737,#19738,#19739,#19740,#19741,#19742,#19743,
#19744,#19745,#19746,#19747,#19748,#19749),.UNSPECIFIED.,.F.,.F.,(4,2,2,
2,2,2,2,2,2,2,4),(0.0591825211272536,0.157966726598481,0.236950089897721,
0.315933453196962,0.391576304923761,0.46721915665056,0.542862008377359,
0.618504860104159,0.697488223403399,0.776471586702639,0.875255792173867),
 .UNSPECIFIED.);
#417=B_SPLINE_CURVE_WITH_KNOTS('',3,(#19899,#19900,#19901,#19902,#19903,
#19904,#19905,#19906,#19907,#19908,#19909,#19910,#19911,#19912,#19913,#19914,
#19915,#19916,#19917,#19918,#19919,#19920),.UNSPECIFIED.,.F.,.F.,(4,2,2,
2,2,2,2,2,2,2,4),(0.0789094028588958,0.210573405340968,0.315860108011452,
0.421146810681936,0.522142632548711,0.623138454415485,0.72413427628226,
0.825130098149035,0.930416800819519,1.03570350349,1.16736750597208),
 .UNSPECIFIED.);
#418=B_SPLINE_CURVE_WITH_KNOTS('',3,(#19924,#19925,#19926,#19927,#19928,
#19929,#19930,#19931,#19932,#19933,#19934,#19935,#19936,#19937,#19938,#19939,
#19940,#19941,#19942,#19943,#19944,#19945),.UNSPECIFIED.,.F.,.F.,(4,2,2,
2,2,2,2,2,2,2,4),(0.0774793363974613,0.142088896491891,0.284177792983782,
0.411119756996526,0.514392970548519,0.617666184100513,0.720939397652506,
0.8242126112045,0.951154575217244,1.09324347170913,1.15785303180356),
 .UNSPECIFIED.);
#419=B_SPLINE_CURVE_WITH_KNOTS('',3,(#19951,#19952,#19953,#19954,#19955,
#19956,#19957,#19958,#19959,#19960,#19961,#19962,#19963,#19964,#19965,#19966,
#19967,#19968,#19969,#19970,#19971,#19972),.UNSPECIFIED.,.F.,.F.,(4,2,2,
2,2,2,2,2,2,2,4),(0.0774793363974613,0.142088896491891,0.284177792983782,
0.411119756996525,0.514392970548519,0.617666184100513,0.720939397652506,
0.8242126112045,0.951154575217243,1.09324347170913,1.15785303180356),
 .UNSPECIFIED.);
#420=B_SPLINE_CURVE_WITH_KNOTS('',3,(#19976,#19977,#19978,#19979,#19980,
#19981,#19982,#19983,#19984,#19985,#19986,#19987,#19988,#19989,#19990,#19991,
#19992,#19993,#19994,#19995,#19996,#19997),.UNSPECIFIED.,.F.,.F.,(4,2,2,
2,2,2,2,2,2,2,4),(0.0774793363974614,0.142088896491891,0.284177792983781,
0.411119756996525,0.514392970548519,0.617666184100512,0.720939397652506,
0.824212611204499,0.951154575217243,1.09324347170913,1.15785303180356),
 .UNSPECIFIED.);
#421=B_SPLINE_CURVE_WITH_KNOTS('',3,(#20001,#20002,#20003,#20004,#20005,
#20006,#20007,#20008,#20009,#20010,#20011,#20012),.UNSPECIFIED.,.F.,.F.,
(4,2,2,2,2,4),(0.0774793363974613,0.142088896491891,0.284177792983781,0.411119756996525,
0.514392970548519,0.617666184100512),.UNSPECIFIED.);
#422=B_SPLINE_CURVE_WITH_KNOTS('',3,(#20017,#20018,#20019,#20020,#20021,
#20022,#20023,#20024,#20025,#20026,#20027,#20028),.UNSPECIFIED.,.F.,.F.,
(4,2,2,2,2,4),(0.617666184100512,0.720939397652506,0.824212611204499,0.951154575217243,
1.09324347170913,1.15785303180356),.UNSPECIFIED.);
#423=B_SPLINE_CURVE_WITH_KNOTS('',3,(#20032,#20033,#20034,#20035,#20036,
#20037,#20038,#20039,#20040,#20041,#20042,#20043,#20044,#20045,#20046,#20047,
#20048,#20049,#20050,#20051,#20052,#20053),.UNSPECIFIED.,.F.,.F.,(4,2,2,
2,2,2,2,2,2,2,4),(0.0774793363974613,0.142088896491891,0.284177792983782,
0.411119756996526,0.514392970548519,0.617666184100513,0.720939397652507,
0.8242126112045,0.951154575217245,1.09324347170914,1.15785303180356),
 .UNSPECIFIED.);
#424=B_SPLINE_CURVE_WITH_KNOTS('',3,(#20057,#20058,#20059,#20060,#20061,
#20062,#20063,#20064,#20065,#20066,#20067,#20068,#20069,#20070,#20071,#20072,
#20073,#20074,#20075,#20076,#20077,#20078),.UNSPECIFIED.,.F.,.F.,(4,2,2,
2,2,2,2,2,2,2,4),(0.0774793363974613,0.142088896491891,0.284177792983782,
0.411119756996526,0.514392970548519,0.617666184100513,0.720939397652506,
0.824212611204499,0.951154575217243,1.09324347170913,1.15785303180356),
 .UNSPECIFIED.);
#425=B_SPLINE_CURVE_WITH_KNOTS('',3,(#20082,#20083,#20084,#20085,#20086,
#20087,#20088,#20089,#20090,#20091,#20092,#20093,#20094,#20095,#20096,#20097,
#20098,#20099,#20100,#20101,#20102,#20103),.UNSPECIFIED.,.F.,.F.,(4,2,2,
2,2,2,2,2,2,2,4),(0.0774793363974613,0.142088896491891,0.284177792983782,
0.411119756996526,0.514392970548519,0.617666184100513,0.720939397652506,
0.8242126112045,0.951154575217244,1.09324347170913,1.15785303180356),
 .UNSPECIFIED.);
#426=B_SPLINE_CURVE_WITH_KNOTS('',3,(#20107,#20108,#20109,#20110,#20111,
#20112,#20113,#20114,#20115,#20116,#20117,#20118,#20119,#20120,#20121,#20122,
#20123,#20124,#20125,#20126,#20127,#20128),.UNSPECIFIED.,.F.,.F.,(4,2,2,
2,2,2,2,2,2,2,4),(0.0774793363974613,0.142088896491891,0.284177792983782,
0.411119756996526,0.514392970548519,0.617666184100513,0.720939397652506,
0.8242126112045,0.951154575217243,1.09324347170913,1.15785303180356),
 .UNSPECIFIED.);
#427=B_SPLINE_CURVE_WITH_KNOTS('',3,(#20136,#20137,#20138,#20139,#20140,
#20141,#20142,#20143,#20144,#20145,#20146,#20147,#20148,#20149,#20150,#20151,
#20152,#20153,#20154,#20155,#20156,#20157),.UNSPECIFIED.,.F.,.F.,(4,2,2,
2,2,2,2,2,2,2,4),(0.0789094028588958,0.210573405340968,0.315860108011452,
0.421146810681936,0.522142632548711,0.623138454415485,0.72413427628226,
0.825130098149035,0.930416800819519,1.03570350349,1.16736750597208),
 .UNSPECIFIED.);
#428=B_SPLINE_CURVE_WITH_KNOTS('',3,(#20165,#20166,#20167,#20168,#20169,
#20170,#20171,#20172,#20173,#20174,#20175,#20176,#20177,#20178,#20179,#20180,
#20181,#20182,#20183,#20184,#20185,#20186),.UNSPECIFIED.,.F.,.F.,(4,2,2,
2,2,2,2,2,2,2,4),(0.0789094028588958,0.210573405340969,0.315860108011453,
0.421146810681937,0.522142632548712,0.623138454415486,0.724134276282261,
0.825130098149035,0.930416800819519,1.03570350349,1.16736750597208),
 .UNSPECIFIED.);
#429=B_SPLINE_CURVE_WITH_KNOTS('',3,(#20195,#20196,#20197,#20198,#20199,
#20200,#20201,#20202,#20203,#20204,#20205,#20206),.UNSPECIFIED.,.F.,.F.,
(4,2,2,2,2,4),(0.0789094028588958,0.210573405340968,0.315860108011452,0.421146810681937,
0.522142632548711,0.623138454415486),.UNSPECIFIED.);
#430=B_SPLINE_CURVE_WITH_KNOTS('',3,(#20208,#20209,#20210,#20211,#20212,
#20213,#20214,#20215,#20216,#20217,#20218,#20219),.UNSPECIFIED.,.F.,.F.,
(4,2,2,2,2,4),(0.623138454415486,0.72413427628226,0.825130098149035,0.930416800819519,
1.03570350349,1.16736750597208),.UNSPECIFIED.);
#431=B_SPLINE_CURVE_WITH_KNOTS('',3,(#20226,#20227,#20228,#20229,#20230,
#20231,#20232,#20233,#20234,#20235,#20236,#20237,#20238,#20239,#20240,#20241,
#20242,#20243,#20244,#20245,#20246,#20247),.UNSPECIFIED.,.F.,.F.,(4,2,2,
2,2,2,2,2,2,2,4),(0.0789094028588958,0.210573405340968,0.315860108011452,
0.421146810681936,0.522142632548711,0.623138454415486,0.72413427628226,
0.825130098149035,0.930416800819519,1.03570350349,1.16736750597208),
 .UNSPECIFIED.);
#432=B_SPLINE_CURVE_WITH_KNOTS('',3,(#20255,#20256,#20257,#20258,#20259,
#20260,#20261,#20262,#20263,#20264,#20265,#20266,#20267,#20268,#20269,#20270,
#20271,#20272,#20273,#20274,#20275,#20276),.UNSPECIFIED.,.F.,.F.,(4,2,2,
2,2,2,2,2,2,2,4),(0.0789094028588957,0.210573405340968,0.315860108011452,
0.421146810681936,0.522142632548711,0.623138454415485,0.72413427628226,
0.825130098149035,0.930416800819519,1.03570350349,1.16736750597207),
 .UNSPECIFIED.);
#433=B_SPLINE_CURVE_WITH_KNOTS('',3,(#20284,#20285,#20286,#20287,#20288,
#20289,#20290,#20291,#20292,#20293,#20294,#20295,#20296,#20297,#20298,#20299,
#20300,#20301,#20302,#20303,#20304,#20305),.UNSPECIFIED.,.F.,.F.,(4,2,2,
2,2,2,2,2,2,2,4),(0.0789094028588958,0.210573405340968,0.315860108011452,
0.421146810681936,0.522142632548711,0.623138454415486,0.72413427628226,
0.825130098149035,0.930416800819519,1.03570350349,1.16736750597208),
 .UNSPECIFIED.);
#434=B_SPLINE_CURVE_WITH_KNOTS('',3,(#20314,#20315,#20316,#20317,#20318,
#20319,#20320,#20321,#20322,#20323,#20324,#20325,#20326,#20327,#20328,#20329,
#20330,#20331,#20332,#20333,#20334,#20335),.UNSPECIFIED.,.F.,.F.,(4,2,2,
2,2,2,2,2,2,2,4),(0.0789094028588958,0.210573405340968,0.315860108011452,
0.421146810681936,0.522142632548711,0.623138454415485,0.72413427628226,
0.825130098149035,0.930416800819519,1.03570350349,1.16736750597208),
 .UNSPECIFIED.);
#435=B_SPLINE_CURVE_WITH_KNOTS('',3,(#21347,#21348,#21349,#21350,#21351,
#21352,#21353,#21354,#21355,#21356,#21357,#21358,#21359,#21360,#21361,#21362,
#21363,#21364,#21365,#21366,#21367,#21368,#21369,#21370,#21371),
 .UNSPECIFIED.,.F.,.F.,(4,3,3,3,3,3,3,3,4),(-3.56038179279204,-3.46201024481372,
-2.96743735269747,-2.47286446058123,-1.97829156846498,-1.48371867634874,
-0.989145784232491,-0.494572892116246,0.),.UNSPECIFIED.);
#436=B_SPLINE_CURVE_WITH_KNOTS('',3,(#21374,#21375,#21376,#21377,#21378,
#21379,#21380,#21381,#21382,#21383,#21384,#21385,#21386,#21387,#21388,#21389,
#21390,#21391,#21392,#21393,#21394,#21395,#21396,#21397,#21398,#21399,#21400,
#21401,#21402,#21403,#21404,#21405,#21406,#21407,#21408,#21409,#21410,#21411,
#21412,#21413),.UNSPECIFIED.,.F.,.F.,(4,3,3,3,3,3,3,3,3,3,3,3,3,4),(0.937891254796418,
0.989145784232494,1.48371867634874,1.97829156846498,2.47286446058123,2.96743735269748,
3.46201024481372,3.95658313692997,4.45115602904621,4.94572892116246,5.44030181327871,
5.93487470539495,6.42944759751119,6.80228742277363),.UNSPECIFIED.);
#437=B_SPLINE_CURVE_WITH_KNOTS('',3,(#21418,#21419,#21420,#21421,#21422,
#21423,#21424,#21425,#21426,#21427,#21428,#21429,#21430,#21431,#21432,#21433,
#21434,#21435,#21436,#21437,#21438,#21439,#21440,#21441,#21442,#21443,#21444,
#21445,#21446,#21447,#21448,#21449,#21450,#21451,#21452,#21453,#21454,#21455,
#21456,#21457),.UNSPECIFIED.,.F.,.F.,(4,3,3,3,3,3,3,3,3,3,3,3,3,4),(-9.8435670999716,
-9.39688495020867,-8.90231205809242,-8.40773916597618,-7.91316627385993,
-7.41859338174369,-6.92402048962744,-6.42944759751119,-5.93487470539495,
-5.4403018132787,-4.94572892116246,-4.45115602904621,-3.95658313692996,
-3.56038179279204),.UNSPECIFIED.);
#438=B_SPLINE_CURVE_WITH_KNOTS('',3,(#21458,#21459,#21460,#21461,#21462,
#21463,#21464,#21465,#21466,#21467,#21468,#21469,#21470,#21471,#21472,#21473,
#21474,#21475,#21476,#21477,#21478,#21479,#21480,#21481,#21482,#21483,#21484,
#21485,#21486,#21487,#21488,#21489,#21490,#21491,#21492,#21493,#21494,#21495,
#21496,#21497,#21498,#21499,#21500),.UNSPECIFIED.,.F.,.F.,(4,3,3,3,3,3,
3,3,3,3,3,3,3,3,4),(6.80228742277363,6.92402048962744,7.41859338174369,
7.91316627385993,8.40773916597617,8.90231205809242,9.39688495020867,9.89145784232491,
10.3860307344412,10.8806036265574,11.3751765186736,11.8697494107899,12.3643223029061,
12.8588951950224,13.0854727299532),.UNSPECIFIED.);
#439=B_SPLINE_CURVE_WITH_KNOTS('',3,(#21505,#21506,#21507,#21508,#21509,
#21510,#21511,#21512,#21513,#21514,#21515,#21516,#21517,#21518,#21519,#21520,
#21521,#21522,#21523,#21524,#21525,#21526,#21527,#21528,#21529,#21530,#21531,
#21532,#21533,#21534,#21535,#21536,#21537,#21538,#21539,#21540,#21541,#21542,
#21543,#21544,#21545,#21546,#21547),.UNSPECIFIED.,.F.,.F.,(4,3,3,3,3,3,
3,3,3,3,3,3,3,3,4),(-16.1267524071512,-15.8263325477199,-15.3317596556036,
-14.8371867634874,-14.3426138713711,-13.8480409792549,-13.3534680871386,
-12.8588951950224,-12.3643223029061,-11.8697494107899,-11.3751765186736,
-10.8806036265574,-10.3860307344412,-9.89145784232491,-9.8435670999716),
 .UNSPECIFIED.);
#440=B_SPLINE_CURVE_WITH_KNOTS('',3,(#21548,#21549,#21550,#21551,#21552,
#21553,#21554,#21555,#21556,#21557,#21558,#21559,#21560,#21561,#21562,#21563,
#21564,#21565,#21566,#21567,#21568,#21569,#21570,#21571,#21572,#21573,#21574,
#21575,#21576,#21577,#21578,#21579,#21580,#21581,#21582,#21583,#21584,#21585,
#21586,#21587,#21588,#21589,#21590),.UNSPECIFIED.,.F.,.F.,(4,3,3,3,3,3,
3,3,3,3,3,3,3,3,4),(13.0854727299532,13.3534680871386,13.8480409792549,
14.3426138713711,14.8371867634874,15.3317596556036,15.8263325477199,16.3209054398361,
16.8154783319523,17.3100512240686,17.8046241161848,18.2991970083011,18.7937699004173,
19.2883427925336,19.3686580371328),.UNSPECIFIED.);
#441=B_SPLINE_CURVE_WITH_KNOTS('',3,(#21595,#21596,#21597,#21598,#21599,
#21600,#21601,#21602,#21603,#21604,#21605,#21606,#21607,#21608,#21609,#21610,
#21611,#21612,#21613,#21614,#21615,#21616,#21617,#21618,#21619,#21620,#21621,
#21622,#21623,#21624,#21625,#21626,#21627,#21628,#21629,#21630,#21631,#21632,
#21633,#21634,#21635,#21636,#21637),.UNSPECIFIED.,.F.,.F.,(4,3,3,3,3,3,
3,3,3,3,3,3,3,3,4),(-22.4099377143308,-22.2557801452311,-21.7612072531148,
-21.2666343609986,-20.7720614688823,-20.2774885767661,-19.7829156846498,
-19.2883427925336,-18.7937699004173,-18.2991970083011,-17.8046241161848,
-17.3100512240686,-16.8154783319523,-16.3209054398361,-16.1267524071512),
 .UNSPECIFIED.);
#442=B_SPLINE_CURVE_WITH_KNOTS('',3,(#21638,#21639,#21640,#21641,#21642,
#21643,#21644,#21645,#21646,#21647,#21648,#21649,#21650,#21651,#21652,#21653,
#21654,#21655,#21656,#21657,#21658,#21659,#21660,#21661,#21662,#21663,#21664,
#21665,#21666,#21667,#21668,#21669,#21670,#21671,#21672,#21673,#21674,#21675,
#21676,#21677),.UNSPECIFIED.,.F.,.F.,(4,3,3,3,3,3,3,3,3,3,3,3,3,4),(19.3686580371328,
19.7829156846498,20.2774885767661,20.7720614688823,21.2666343609986,21.7612072531148,
22.255780145231,22.7503530373473,23.2449259294635,23.7394988215798,24.234071713696,
24.7286446058123,25.2232174979285,25.6518433443124),.UNSPECIFIED.);
#443=B_SPLINE_CURVE_WITH_KNOTS('',3,(#21682,#21683,#21684,#21685,#21686,
#21687,#21688,#21689,#21690,#21691,#21692,#21693,#21694,#21695,#21696,#21697,
#21698,#21699,#21700,#21701,#21702,#21703,#21704,#21705,#21706,#21707,#21708,
#21709,#21710,#21711,#21712,#21713,#21714,#21715,#21716,#21717,#21718,#21719,
#21720,#21721,#21722,#21723,#21724),.UNSPECIFIED.,.F.,.F.,(4,3,3,3,3,3,
3,3,3,3,3,3,3,3,4),(-28.6931230215104,-28.6852277427422,-28.190654850626,
-27.6960819585097,-27.2015090663935,-26.7069361742773,-26.212363282161,
-25.7177903900448,-25.2232174979285,-24.7286446058123,-24.234071713696,
-23.7394988215798,-23.2449259294635,-22.7503530373473,-22.4099377143308),
 .UNSPECIFIED.);
#444=B_SPLINE_CURVE_WITH_KNOTS('',3,(#21725,#21726,#21727,#21728,#21729,
#21730,#21731,#21732,#21733,#21734,#21735,#21736,#21737,#21738,#21739,#21740,
#21741,#21742,#21743,#21744,#21745,#21746,#21747,#21748,#21749,#21750,#21751,
#21752,#21753,#21754,#21755,#21756,#21757,#21758,#21759,#21760,#21761,#21762,
#21763,#21764,#21765,#21766,#21767),.UNSPECIFIED.,.F.,.F.,(4,3,3,3,3,3,
3,3,3,3,3,3,3,3,4),(25.6518433443124,25.7177903900448,26.212363282161,26.7069361742773,
27.2015090663935,27.6960819585097,28.190654850626,28.6852277427422,29.1798006348585,
29.6743735269747,30.168946419091,30.6635193112072,31.1580922033235,31.6526650954397,
31.935028651492),.UNSPECIFIED.);
#445=B_SPLINE_CURVE_WITH_KNOTS('',3,(#21772,#21773,#21774,#21775,#21776,
#21777,#21778,#21779,#21780,#21781,#21782,#21783,#21784,#21785,#21786,#21787,
#21788,#21789,#21790,#21791,#21792,#21793,#21794,#21795,#21796,#21797,#21798,
#21799,#21800,#21801,#21802,#21803,#21804,#21805,#21806,#21807,#21808,#21809,
#21810,#21811),.UNSPECIFIED.,.F.,.F.,(4,3,3,3,3,3,3,3,3,3,3,3,3,4),(-34.97630832869,
-34.6201024481372,-34.1255295560209,-33.6309566639047,-33.1363837717884,
-32.6418108796722,-32.147237987556,-31.6526650954397,-31.1580922033235,
-30.6635193112072,-30.168946419091,-29.6743735269747,-29.1798006348585,
-28.6931230215104),.UNSPECIFIED.);
#446=B_SPLINE_CURVE_WITH_KNOTS('',3,(#21812,#21813,#21814,#21815,#21816,
#21817,#21818,#21819,#21820,#21821,#21822,#21823,#21824,#21825,#21826,#21827,
#21828,#21829,#21830,#21831,#21832,#21833,#21834,#21835,#21836,#21837,#21838,
#21839,#21840,#21841,#21842,#21843,#21844,#21845,#21846,#21847,#21848,#21849,
#21850,#21851,#21852,#21853,#21854),.UNSPECIFIED.,.F.,.F.,(4,3,3,3,3,3,
3,3,3,3,3,3,3,3,4),(31.935028651492,32.147237987556,32.6418108796722,33.1363837717885,
33.6309566639047,34.1255295560209,34.6201024481372,35.1146753402534,35.6092482323697,
36.1038211244859,36.5983940166022,37.0929669087184,37.5875398008347,38.0821126929509,
38.2182139586716),.UNSPECIFIED.);
#447=B_SPLINE_CURVE_WITH_KNOTS('',3,(#21859,#21860,#21861,#21862,#21863,
#21864,#21865,#21866,#21867,#21868,#21869,#21870,#21871,#21872,#21873,#21874,
#21875,#21876,#21877,#21878,#21879,#21880,#21881,#21882,#21883,#21884,#21885,
#21886,#21887,#21888,#21889,#21890,#21891,#21892,#21893,#21894,#21895,#21896,
#21897,#21898,#21899,#21900,#21901),.UNSPECIFIED.,.F.,.F.,(4,3,3,3,3,3,
3,3,3,3,3,3,3,3,4),(-41.2594936358696,-41.0495500456484,-40.5549771535321,
-40.0604042614159,-39.5658313692996,-39.0712584771834,-38.5766855850671,
-38.0821126929509,-37.5875398008347,-37.0929669087184,-36.5983940166022,
-36.1038211244859,-35.6092482323697,-35.1146753402534,-34.97630832869),
 .UNSPECIFIED.);
#448=B_SPLINE_CURVE_WITH_KNOTS('',3,(#21902,#21903,#21904,#21905,#21906,
#21907,#21908,#21909,#21910,#21911,#21912,#21913,#21914,#21915,#21916,#21917,
#21918,#21919,#21920,#21921,#21922,#21923,#21924,#21925,#21926,#21927,#21928,
#21929,#21930,#21931,#21932,#21933,#21934,#21935,#21936,#21937,#21938,#21939,
#21940,#21941),.UNSPECIFIED.,.F.,.F.,(4,3,3,3,3,3,3,3,3,3,3,3,3,4),(38.2182139586716,
38.5766855850671,39.0712584771834,39.5658313692996,40.0604042614159,40.5549771535321,
41.0495500456484,41.5441229377646,42.0386958298809,42.5332687219971,43.0278416141134,
43.5224145062296,44.0169873983459,44.5013992658512),.UNSPECIFIED.);
#449=B_SPLINE_CURVE_WITH_KNOTS('',3,(#21946,#21947,#21948,#21949,#21950,
#21951,#21952,#21953,#21954,#21955,#21956,#21957,#21958,#21959,#21960,#21961,
#21962,#21963,#21964,#21965,#21966,#21967,#21968,#21969,#21970,#21971,#21972,
#21973,#21974,#21975,#21976,#21977,#21978,#21979,#21980,#21981,#21982,#21983,
#21984,#21985,#21986,#21987,#21988),.UNSPECIFIED.,.F.,.F.,(4,3,3,3,3,3,
3,3,3,3,3,3,3,3,4),(-47.5426789430491,-47.4789976431596,-46.9844247510433,
-46.4898518589271,-45.9952789668108,-45.5007060746946,-45.0061331825783,
-44.5115602904621,-44.0169873983458,-43.5224145062296,-43.0278416141134,
-42.5332687219971,-42.0386958298809,-41.5441229377646,-41.2594936358696),
 .UNSPECIFIED.);
#450=B_SPLINE_CURVE_WITH_KNOTS('',3,(#21989,#21990,#21991,#21992,#21993,
#21994,#21995,#21996,#21997,#21998,#21999,#22000,#22001,#22002,#22003,#22004,
#22005,#22006,#22007,#22008,#22009,#22010,#22011,#22012,#22013,#22014,#22015,
#22016,#22017,#22018,#22019,#22020,#22021,#22022,#22023,#22024,#22025,#22026,
#22027,#22028,#22029,#22030,#22031),.UNSPECIFIED.,.F.,.F.,(4,3,3,3,3,3,
3,3,3,3,3,3,3,3,4),(44.5013992658512,44.5115602904621,45.0061331825783,
45.5007060746946,45.9952789668108,46.4898518589271,46.9844247510433,47.4789976431596,
47.9735705352758,48.4681434273921,48.9627163195083,49.4572892116245,49.9518621037408,
50.446434995857,50.7845845730308),.UNSPECIFIED.);
#451=B_SPLINE_CURVE_WITH_KNOTS('',3,(#22038,#22039,#22040,#22041,#22042,
#22043,#22044,#22045,#22046,#22047),.UNSPECIFIED.,.F.,.F.,(4,3,3,4),(-54.4542726622231,
-54.403018132787,-53.9084452406708,-53.8258642502287),.UNSPECIFIED.);
#452=B_SPLINE_CURVE_WITH_KNOTS('',3,(#22053,#22054,#22055,#22056,#22057,
#22058,#22059),.UNSPECIFIED.,.F.,.F.,(4,1,1,1,4),(65.9734457253856,66.0560267158277,
66.5505996079439,67.0451725000601,67.5397453921764),.UNSPECIFIED.);
#453=B_SPLINE_CURVE_WITH_KNOTS('',3,(#22062,#22063,#22064,#22065,#22066,
#22067,#22068,#22069,#22070,#22071,#22072,#22073),.UNSPECIFIED.,.F.,.F.,
(4,1,1,1,1,1,1,1,1,4),(65.9734457253856,66.1298690403281,66.6244419324444,
67.1190148245607,67.6135877166769,68.1081606087931,68.6027335009094,69.0973063930256,
69.5918792851419,69.643133814578),.UNSPECIFIED.);
#454=B_SPLINE_CURVE_WITH_KNOTS('',3,(#22078,#22079,#22080,#22081,#22082,
#22083,#22084,#22085,#22086,#22087,#22088,#22089,#22090,#22091,#22092,#22093),
 .UNSPECIFIED.,.F.,.F.,(4,1,1,1,1,1,1,1,1,1,1,1,1,4),(59.6902604182061,
60.1211520104327,60.615724902549,61.1102977946652,61.6048706867815,62.0994435788977,
62.5940164710139,63.0885893631302,63.5831622552464,64.0777351473627,64.5723080394789,
65.0668809315952,65.5614538237114,65.9734457253856),.UNSPECIFIED.);
#455=B_SPLINE_CURVE_WITH_KNOTS('',3,(#22094,#22095,#22096,#22097,#22098,
#22099,#22100,#22101,#22102,#22103,#22104,#22105,#22106,#22107,#22108,#22109,
#22110),.UNSPECIFIED.,.F.,.F.,(4,1,1,1,1,1,1,1,1,1,1,1,1,1,4),(59.6902604182061,
59.700421442817,60.1949943349332,60.6895672270495,61.1841401191657,61.6787130112819,
62.1732859033982,62.6678587955144,63.1624316876307,63.6570045797469,64.1515774718632,
64.6461503639794,65.1407232560957,65.6352961482119,65.9734457253856),
 .UNSPECIFIED.);
#456=B_SPLINE_CURVE_WITH_KNOTS('',3,(#22115,#22116,#22117,#22118,#22119,
#22120,#22121,#22122,#22123,#22124,#22125,#22126,#22127,#22128,#22129,#22130,
#22131),.UNSPECIFIED.,.F.,.F.,(4,1,1,1,1,1,1,1,1,1,1,1,1,1,4),(53.4070751110264,
53.6917044129215,54.1862773050378,54.680850197154,55.1754230892703,55.6699959813865,
56.1645688735028,56.659141765619,57.1537146577353,57.6482875498515,58.1428604419677,
58.637433334084,59.1320062262002,59.6265791183165,59.6902604182061),
 .UNSPECIFIED.);
#457=B_SPLINE_CURVE_WITH_KNOTS('',3,(#22132,#22133,#22134,#22135,#22136,
#22137,#22138,#22139,#22140,#22141,#22142,#22143,#22144,#22145,#22146,#22147),
 .UNSPECIFIED.,.F.,.F.,(4,1,1,1,1,1,1,1,1,1,1,1,1,4),(53.4070751110264,
53.765546737422,54.2601196295383,54.7546925216545,55.2492654137708,55.743838305887,
56.2384111980032,56.7329840901195,57.2275569822357,57.722129874352,58.2167027664682,
58.7112756585845,59.2058485507007,59.6902604182061),.UNSPECIFIED.);
#458=B_SPLINE_CURVE_WITH_KNOTS('',3,(#22152,#22153,#22154,#22155,#22156,
#22157,#22158,#22159,#22160,#22161,#22162,#22163,#22164,#22165,#22166,#22167,
#22168),.UNSPECIFIED.,.F.,.F.,(4,1,1,1,1,1,1,1,1,1,1,1,1,1,4),(47.1238898038469,
47.2622568154103,47.7568297075266,48.2514025996428,48.7459754917591,49.2405483838753,
49.7351212759916,50.2296941681078,50.7242670602241,51.2188399523403,51.7134128444565,
52.2079857365728,52.702558628689,53.1971315208053,53.4070751110264),
 .UNSPECIFIED.);
#459=B_SPLINE_CURVE_WITH_KNOTS('',3,(#22169,#22170,#22171,#22172,#22173,
#22174,#22175,#22176,#22177,#22178,#22179,#22180,#22181,#22182,#22183,#22184,
#22185),.UNSPECIFIED.,.F.,.F.,(4,1,1,1,1,1,1,1,1,1,1,1,1,1,4),(47.1238898038469,
47.3360991399108,47.8306720320271,48.3252449241433,48.8198178162596,49.3143907083758,
49.8089636004921,50.3035364926083,50.7981093847245,51.2926822768408,51.787255168957,
52.2818280610733,52.7764009531895,53.2709738453058,53.4070751110264),
 .UNSPECIFIED.);
#460=B_SPLINE_CURVE_WITH_KNOTS('',3,(#22190,#22191,#22192,#22193,#22194,
#22195,#22196,#22197,#22198,#22199,#22200,#22201,#22202,#22203,#22204,#22205),
 .UNSPECIFIED.,.F.,.F.,(4,1,1,1,1,1,1,1,1,1,1,1,1,4),(40.8407044966673,
41.3273821100154,41.8219550021316,42.3165278942479,42.8111007863641,43.3056736784804,
43.8002465705966,44.2948194627129,44.7893923548291,45.2839652469454,45.7785381390616,
46.2731110311778,46.7676839232941,47.1238898038469),.UNSPECIFIED.);
#461=B_SPLINE_CURVE_WITH_KNOTS('',3,(#22206,#22207,#22208,#22209,#22210,
#22211,#22212,#22213,#22214,#22215,#22216,#22217,#22218,#22219,#22220,#22221,
#22222),.UNSPECIFIED.,.F.,.F.,(4,1,1,1,1,1,1,1,1,1,1,1,1,1,4),(40.8407044966673,
40.9066515423996,41.4012244345159,41.8957973266321,42.3903702187484,42.8849431108646,
43.3795160029809,43.8740888950971,44.3686617872134,44.8632346793296,45.3578075714458,
45.8523804635621,46.3469533556783,46.8415262477946,47.1238898038469),
 .UNSPECIFIED.);
#462=B_SPLINE_CURVE_WITH_KNOTS('',3,(#22227,#22228,#22229,#22230,#22231,
#22232,#22233,#22234,#22235,#22236,#22237,#22238,#22239,#22240,#22241,#22242,
#22243),.UNSPECIFIED.,.F.,.F.,(4,1,1,1,1,1,1,1,1,1,1,1,1,1,4),(34.5575191894877,
34.8979345125042,35.3925074046204,35.8870802967367,36.3816531888529,36.8762260809692,
37.3707989730854,37.8653718652017,38.3599447573179,38.8545176494342,39.3490905415504,
39.8436634336667,40.3382363257829,40.8328092178991,40.8407044966673),
 .UNSPECIFIED.);
#463=B_SPLINE_CURVE_WITH_KNOTS('',3,(#22244,#22245,#22246,#22247,#22248,
#22249,#22250,#22251,#22252,#22253,#22254,#22255,#22256,#22257,#22258,#22259),
 .UNSPECIFIED.,.F.,.F.,(4,1,1,1,1,1,1,1,1,1,1,1,1,4),(34.5575191894877,
34.9717768370047,35.4663497291209,35.9609226212372,36.4554955133534,36.9500684054697,
37.4446412975859,37.9392141897022,38.4337870818184,38.9283599739347,39.4229328660509,
39.9175057581671,40.4120786502834,40.8407044966673),.UNSPECIFIED.);
#464=B_SPLINE_CURVE_WITH_KNOTS('',3,(#22264,#22265,#22266,#22267,#22268,
#22269,#22270,#22271,#22272,#22273,#22274,#22275,#22276,#22277,#22278,#22279,
#22280),.UNSPECIFIED.,.F.,.F.,(4,1,1,1,1,1,1,1,1,1,1,1,1,1,4),(28.2743338823081,
28.468486914993,28.9630598071093,29.4576326992255,29.9522055913417,30.446778483458,
30.9413513755742,31.4359242676905,31.9304971598067,32.425070051923,32.9196429440392,
33.4142158361555,33.9087887282717,34.403361620388,34.5575191894877),
 .UNSPECIFIED.);
#465=B_SPLINE_CURVE_WITH_KNOTS('',3,(#22281,#22282,#22283,#22284,#22285,
#22286,#22287,#22288,#22289,#22290,#22291,#22292,#22293,#22294,#22295,#22296,
#22297),.UNSPECIFIED.,.F.,.F.,(4,1,1,1,1,1,1,1,1,1,1,1,1,1,4),(28.2743338823081,
28.5423292394935,29.0369021316097,29.531475023726,30.0260479158422,30.5206208079585,
31.0151937000747,31.509766592191,32.0043394843072,32.4989123764235,32.9934852685397,
33.488058160656,33.9826310527722,34.4772039448884,34.5575191894877),
 .UNSPECIFIED.);
#466=B_SPLINE_CURVE_WITH_KNOTS('',3,(#22302,#22303,#22304,#22305,#22306,
#22307,#22308,#22309,#22310,#22311,#22312,#22313,#22314,#22315,#22316,#22317,
#22318),.UNSPECIFIED.,.F.,.F.,(4,1,1,1,1,1,1,1,1,1,1,1,1,1,4),(21.9911485751285,
22.0390393174818,22.5336122095981,23.0281851017143,23.5227579938306,24.0173308859468,
24.511903778063,25.0064766701793,25.5010495622955,25.9956224544118,26.490195346528,
26.9847682386443,27.4793411307605,27.9739140228768,28.2743338823081),
 .UNSPECIFIED.);
#467=B_SPLINE_CURVE_WITH_KNOTS('',3,(#22319,#22320,#22321,#22322,#22323,
#22324,#22325,#22326,#22327,#22328,#22329,#22330,#22331,#22332,#22333,#22334,
#22335),.UNSPECIFIED.,.F.,.F.,(4,1,1,1,1,1,1,1,1,1,1,1,1,1,4),(21.9911485751285,
22.1128816419823,22.6074545340986,23.1020274262148,23.596600318331,24.0911732104473,
24.5857461025635,25.0803189946798,25.574891886796,26.0694647789123,26.5640376710285,
27.0586105631448,27.553183455261,28.0477563473773,28.2743338823081),
 .UNSPECIFIED.);
#468=B_SPLINE_CURVE_WITH_KNOTS('',3,(#22341,#22342,#22343,#22344,#22345),
 .UNSPECIFIED.,.F.,.F.,(4,1,4),(15.1888611523549,15.6834340444711,15.7079632679489),
 .UNSPECIFIED.);
#469=B_SPLINE_CURVE_WITH_KNOTS('',3,(#22348,#22349,#22350,#22351,#22352,
#22353,#22354,#22355,#22356,#22357),.UNSPECIFIED.,.F.,.F.,(4,1,1,1,1,1,
1,4),(13.0854727299533,13.1367272593894,13.6313001515056,14.1258730436219,
14.6204459357381,15.1150188278544,15.6095917199706,15.7079632679489),
 .UNSPECIFIED.);
#470=B_SPLINE_CURVE_WITH_KNOTS('',3,(#22359,#22360,#22361,#22362,#22363,
#22364,#22365,#22366,#22367,#22368,#22369,#22370,#22371,#22372,#22373,#22374),
 .UNSPECIFIED.,.F.,.F.,(4,1,1,1,1,1,1,1,1,1,1,1,1,4),(15.7079632679489,
16.1041646120869,16.5987375042031,17.0933103963194,17.5878832884356,18.0824561805519,
18.5770290726681,19.0716019647843,19.5661748569006,20.0607477490168,20.5553206411331,
21.0498935332493,21.5444664253656,21.9911485751285),.UNSPECIFIED.);
#471=B_SPLINE_CURVE_WITH_KNOTS('',3,(#22375,#22376,#22377,#22378,#22379,
#22380,#22381,#22382,#22383,#22384,#22385,#22386,#22387,#22388,#22389,#22390),
 .UNSPECIFIED.,.F.,.F.,(4,1,1,1,1,1,1,1,1,1,1,1,1,4),(15.7079632679489,
16.1780069365874,16.6725798287036,17.1671527208199,17.6617256129361,18.1562985050523,
18.6508713971686,19.1454442892848,19.6400171814011,20.1345900735173,20.6291629656336,
21.1237358577498,21.6183087498661,21.9911485751285),.UNSPECIFIED.);
#472=B_SPLINE_CURVE_WITH_KNOTS('',3,(#22851,#22852,#22853,#22854,#22855,
#22856,#22857,#22858,#22859,#22860,#22861,#22862,#22863,#22864,#22865,#22866,
#22867,#22868,#22869,#22870,#22871,#22872,#22873,#22874,#22875,#22876,#22877,
#22878,#22879,#22880,#22881),.UNSPECIFIED.,.F.,.F.,(4,3,3,3,3,3,3,3,3,3,
4),(0.,0.0822466706468383,0.162608105240606,0.216579893838171,0.23924274204394,
0.301838371937517,0.36076250940623,0.388067588559334,0.409537377502954,
0.476290104322315,0.53753492181237),.UNSPECIFIED.);
#473=B_SPLINE_CURVE_WITH_KNOTS('',3,(#22882,#22883,#22884,#22885,#22886,
#22887,#22888,#22889,#22890,#22891,#22892,#22893,#22894,#22895,#22896,#22897,
#22898,#22899,#22900,#22901,#22902,#22903,#22904,#22905,#22906,#22907,#22908,
#22909),.UNSPECIFIED.,.F.,.F.,(4,3,3,3,3,3,3,3,3,4),(0.,0.0665230127441691,
0.13429495842692,0.176258819244205,0.195926107024299,0.263526952009386,
0.33682854572103,0.365338415901403,0.449700157257057,0.534061898612711),
 .UNSPECIFIED.);
#474=B_SPLINE_CURVE_WITH_KNOTS('',3,(#22910,#22911,#22912,#22913,#22914,
#22915,#22916,#22917,#22918,#22919,#22920,#22921,#22922,#22923,#22924,#22925,
#22926,#22927,#22928,#22929,#22930,#22931,#22932,#22933,#22934,#22935,#22936,
#22937,#22938,#22939,#22940,#22941,#22942,#22943,#22944,#22945,#22946,#22947,
#22948,#22949),.UNSPECIFIED.,.F.,.F.,(4,3,3,3,3,3,3,3,3,3,3,3,3,4),(-53.8258642502287,
-53.4138723485545,-52.9192994564383,-52.424726564322,-51.9301536722058,
-51.4355807800895,-50.9410078879733,-50.446434995857,-49.9518621037408,
-49.4572892116245,-48.9627163195083,-48.4681434273921,-47.9735705352758,
-47.5426789430491),.UNSPECIFIED.);
#475=B_SPLINE_CURVE_WITH_KNOTS('',3,(#23411,#23412,#23413,#23414,#23415,
#23416,#23417,#23418,#23419,#23420,#23421,#23422,#23423,#23424,#23425,#23426,
#23427,#23428,#23429,#23430,#23431,#23432,#23433,#23434,#23435,#23436,#23437,
#23438),.UNSPECIFIED.,.F.,.F.,(4,3,3,3,3,3,3,3,3,4),(0.,0.0665230199567328,
0.134294967830964,0.176258831509978,0.195926124443112,0.263526952009376,
0.336828549458816,0.365338416771381,0.449700157692121,0.534061898612861),
 .UNSPECIFIED.);
#476=B_SPLINE_CURVE_WITH_KNOTS('',3,(#23439,#23440,#23441,#23442,#23443,
#23444,#23445,#23446,#23447,#23448,#23449,#23450,#23451,#23452,#23453,#23454,
#23455,#23456,#23457,#23458,#23459,#23460,#23461,#23462,#23463,#23464,#23465,
#23466,#23467,#23468,#23469),.UNSPECIFIED.,.F.,.F.,(4,3,3,3,3,3,3,3,3,3,
4),(50.7845845730308,50.9410078879733,51.4355807800895,51.9301536722058,
52.424726564322,52.9192994564383,53.4138723485545,53.9084452406708,54.403018132787,
54.8975910249033,55.3921639170195),.UNSPECIFIED.);
#477=B_SPLINE_CURVE_WITH_KNOTS('',3,(#23470,#23471,#23472,#23473,#23474,
#23475,#23476,#23477,#23478,#23479,#23480,#23481,#23482,#23483,#23484,#23485,
#23486,#23487,#23488,#23489,#23490,#23491,#23492,#23493,#23494,#23495,#23496,
#23497,#23498,#23499,#23500),.UNSPECIFIED.,.F.,.F.,(4,3,3,3,3,3,3,3,3,3,
4),(0.,0.0822466663612967,0.162608100396307,0.216579890867136,0.239242742625966,
0.301838371937549,0.360762509406336,0.388067584071394,0.409537375230468,
0.476290092032249,0.537534921812695),.UNSPECIFIED.);
#478=B_SPLINE_CURVE_WITH_KNOTS('',3,(#23709,#23710,#23711,#23712,#23713,
#23714,#23715,#23716,#23717,#23718,#23719,#23720,#23721,#23722,#23723,#23724,
#23725,#23726,#23727),.UNSPECIFIED.,.F.,.F.,(4,3,3,3,3,3,4),(-3.69871549170445,
-3.49775346748116,-2.99807440069814,-2.49839533391511,-1.99871626713209,
-1.49903720034907,-1.00018350866767),.UNSPECIFIED.);
#479=B_SPLINE_CURVE_WITH_KNOTS('',3,(#23730,#23731,#23732,#23733),
 .UNSPECIFIED.,.F.,.F.,(4,4),(0.,0.443060670554495),.UNSPECIFIED.);
#480=B_SPLINE_CURVE_WITH_KNOTS('',3,(#23738,#23739,#23740,#23741,#23742,
#23743,#23744,#23745,#23746,#23747,#23748,#23749,#23750,#23751,#23752,#23753,
#23754,#23755,#23756,#23757,#23758,#23759,#23760,#23761,#23762,#23763,#23764,
#23765,#23766,#23767,#23768,#23769,#23770,#23771,#23772,#23773,#23774,#23775,
#23776,#23777),.UNSPECIFIED.,.F.,.F.,(4,3,3,3,3,3,3,3,3,3,3,3,3,4),(-9.98190079888403,
-9.49390226887744,-8.99422320209442,-8.4945441353114,-7.99486506852837,
-7.49518600174535,-6.99550693496233,-6.4958278681793,-5.99614880139628,
-5.49646973461325,-4.99679066783023,-4.49711160104721,-3.99743253426419,
-3.69871549170445),.UNSPECIFIED.);
#481=B_SPLINE_CURVE_WITH_KNOTS('',3,(#23778,#23779,#23780,#23781,#23782,
#23783,#23784,#23785,#23786,#23787,#23788,#23789,#23790,#23791,#23792,#23793,
#23794,#23795,#23796,#23797,#23798,#23799,#23800,#23801,#23802,#23803,#23804,
#23805,#23806,#23807,#23808,#23809,#23810,#23811,#23812,#23813,#23814,#23815,
#23816,#23817,#23818,#23819,#23820),.UNSPECIFIED.,.F.,.F.,(4,3,3,3,3,3,
3,3,3,3,3,3,3,3,4),(0.443060670554495,0.49967906678306,0.999358133566079,
1.4990372003491,1.99871626713212,2.49839533391514,2.99807440069816,3.49775346748117,
3.99743253426419,4.49711160104721,4.99679066783023,5.49646973461325,5.99614880139627,
6.49582786817929,6.72624597773408),.UNSPECIFIED.);
#482=B_SPLINE_CURVE_WITH_KNOTS('',3,(#23825,#23826,#23827,#23828,#23829,
#23830,#23831,#23832,#23833,#23834,#23835,#23836,#23837,#23838,#23839,#23840,
#23841,#23842,#23843,#23844,#23845,#23846,#23847,#23848,#23849,#23850,#23851,
#23852,#23853,#23854,#23855,#23856,#23857,#23858,#23859,#23860,#23861,#23862,
#23863,#23864,#23865,#23866,#23867),.UNSPECIFIED.,.F.,.F.,(4,3,3,3,3,3,
3,3,3,3,3,3,3,3,4),(-16.2650861060636,-15.9897301370567,-15.4900510702737,
-14.9903720034907,-14.4906929367077,-13.9910138699247,-13.4913348031416,
-12.9916557363586,-12.4919766695756,-11.9922976027926,-11.4926185360095,
-10.9929394692265,-10.4932604024435,-9.99358133566046,-9.98190079888403),
 .UNSPECIFIED.);
#483=B_SPLINE_CURVE_WITH_KNOTS('',3,(#23868,#23869,#23870,#23871,#23872,
#23873,#23874,#23875,#23876,#23877,#23878,#23879,#23880,#23881,#23882,#23883,
#23884,#23885,#23886,#23887,#23888,#23889,#23890,#23891,#23892,#23893,#23894,
#23895,#23896,#23897,#23898,#23899,#23900,#23901,#23902,#23903,#23904,#23905,
#23906,#23907,#23908,#23909,#23910),.UNSPECIFIED.,.F.,.F.,(4,3,3,3,3,3,
3,3,3,3,3,3,3,3,4),(6.72624597773408,6.99550693496231,7.49518600174534,
7.99486506852837,8.49454413531139,8.99422320209442,9.49390226887745,9.99358133566048,
10.4932604024435,10.9929394692265,11.4926185360096,11.9922976027926,12.4919766695756,
12.9916557363586,13.0094312849137),.UNSPECIFIED.);
#484=B_SPLINE_CURVE_WITH_KNOTS('',3,(#23915,#23916,#23917,#23918,#23919,
#23920,#23921,#23922,#23923,#23924,#23925,#23926,#23927,#23928,#23929,#23930,
#23931,#23932,#23933,#23934,#23935,#23936,#23937,#23938,#23939,#23940,#23941,
#23942,#23943,#23944,#23945,#23946,#23947,#23948,#23949,#23950,#23951,#23952,
#23953,#23954,#23955,#23956,#23957),.UNSPECIFIED.,.F.,.F.,(4,3,3,3,3,3,
3,3,3,3,3,3,3,3,4),(-22.5482714132432,-22.485558005236,-21.985878938453,
-21.48619987167,-20.986520804887,-20.486841738104,-19.9871626713209,-19.4874836045379,
-18.9878045377549,-18.4881254709719,-17.9884464041888,-17.4887673374058,
-16.9890882706228,-16.4894092038398,-16.2650861060636),.UNSPECIFIED.);
#485=B_SPLINE_CURVE_WITH_KNOTS('',3,(#23958,#23959,#23960,#23961,#23962,
#23963,#23964,#23965,#23966,#23967,#23968,#23969,#23970,#23971,#23972,#23973,
#23974,#23975,#23976,#23977,#23978,#23979,#23980,#23981,#23982,#23983,#23984,
#23985,#23986,#23987,#23988,#23989,#23990,#23991,#23992,#23993,#23994,#23995,
#23996,#23997),.UNSPECIFIED.,.F.,.F.,(4,3,3,3,3,3,3,3,3,3,3,3,3,4),(13.0094312849137,
13.4913348031417,13.9910138699247,14.4906929367077,14.9903720034907,15.4900510702737,
15.9897301370568,16.4894092038398,16.9890882706228,17.4887673374058,17.9884464041888,
18.4881254709718,18.9878045377549,19.2926165920933),.UNSPECIFIED.);
#486=B_SPLINE_CURVE_WITH_KNOTS('',3,(#24002,#24003,#24004,#24005,#24006,
#24007,#24008,#24009,#24010,#24011,#24012,#24013,#24014,#24015,#24016,#24017,
#24018,#24019,#24020,#24021,#24022,#24023,#24024,#24025,#24026,#24027,#24028,
#24029,#24030,#24031,#24032,#24033,#24034,#24035,#24036,#24037,#24038,#24039,
#24040,#24041),.UNSPECIFIED.,.F.,.F.,(4,3,3,3,3,3,3,3,3,3,3,3,3,4),(-28.8314567204228,
-28.4817068066323,-27.9820277398493,-27.4823486730663,-26.9826696062833,
-26.4829905395002,-25.9833114727172,-25.4836324059342,-24.9839533391512,
-24.4842742723681,-23.9845952055851,-23.4849161388021,-22.9852370720191,
-22.5482714132432),.UNSPECIFIED.);
#487=B_SPLINE_CURVE_WITH_KNOTS('',3,(#24042,#24043,#24044,#24045,#24046,
#24047,#24048,#24049,#24050,#24051,#24052,#24053,#24054,#24055,#24056,#24057,
#24058,#24059,#24060,#24061,#24062,#24063,#24064,#24065,#24066,#24067,#24068,
#24069,#24070,#24071,#24072,#24073,#24074,#24075,#24076,#24077,#24078,#24079,
#24080,#24081,#24082,#24083,#24084),.UNSPECIFIED.,.F.,.F.,(4,3,3,3,3,3,
3,3,3,3,3,3,3,3,4),(19.2926165920933,19.4874836045379,19.9871626713209,
20.4868417381039,20.986520804887,21.48619987167,21.985878938453,22.4855580052361,
22.9852370720191,23.4849161388021,23.9845952055851,24.4842742723682,24.9839533391512,
25.4836324059342,25.5758018992728),.UNSPECIFIED.);
#488=B_SPLINE_CURVE_WITH_KNOTS('',3,(#24089,#24090,#24091,#24092,#24093,
#24094,#24095,#24096,#24097,#24098,#24099,#24100,#24101,#24102,#24103,#24104,
#24105,#24106,#24107,#24108,#24109,#24110,#24111,#24112,#24113,#24114,#24115,
#24116,#24117,#24118,#24119,#24120,#24121,#24122,#24123,#24124,#24125,#24126,
#24127,#24128,#24129,#24130,#24131),.UNSPECIFIED.,.F.,.F.,(4,3,3,3,3,3,
3,3,3,3,3,3,3,3,4),(-35.1146420276024,-34.9775346748116,-34.4778556080286,
-33.9781765412456,-33.4784974744626,-32.9788184076795,-32.4791393408965,
-31.9794602741135,-31.4797812073305,-30.9801021405474,-30.4804230737644,
-29.9807440069814,-29.4810649401984,-28.9813858734153,-28.8314567204228),
 .UNSPECIFIED.);
#489=B_SPLINE_CURVE_WITH_KNOTS('',3,(#24132,#24133,#24134,#24135,#24136,
#24137,#24138,#24139,#24140,#24141,#24142,#24143,#24144,#24145,#24146,#24147,
#24148,#24149,#24150,#24151,#24152,#24153,#24154,#24155,#24156,#24157,#24158,
#24159,#24160,#24161,#24162,#24163,#24164,#24165,#24166,#24167,#24168,#24169,
#24170,#24171),.UNSPECIFIED.,.F.,.F.,(4,3,3,3,3,3,3,3,3,3,3,3,3,4),(25.5758018992728,
25.9833114727172,26.4829905395003,26.9826696062833,27.4823486730663,27.9820277398493,
28.4817068066324,28.9813858734154,29.4810649401984,29.9807440069814,30.4804230737645,
30.9801021405475,31.4797812073305,31.8589872064524),.UNSPECIFIED.);
#490=B_SPLINE_CURVE_WITH_KNOTS('',3,(#24176,#24177,#24178,#24179,#24180,
#24181,#24182,#24183,#24184,#24185,#24186,#24187,#24188,#24189,#24190,#24191,
#24192,#24193,#24194,#24195,#24196,#24197,#24198,#24199,#24200,#24201,#24202,
#24203,#24204,#24205,#24206,#24207,#24208,#24209,#24210,#24211,#24212,#24213,
#24214,#24215),.UNSPECIFIED.,.F.,.F.,(4,3,3,3,3,3,3,3,3,3,3,3,3,4),(-41.397827334782,
-40.9736834762079,-40.4740044094249,-39.9743253426419,-39.4746462758588,
-38.9749672090758,-38.4752881422928,-37.9756090755098,-37.4759300087267,
-36.9762509419437,-36.4765718751607,-35.9768928083777,-35.4772137415947,
-35.1146420276024),.UNSPECIFIED.);
#491=B_SPLINE_CURVE_WITH_KNOTS('',3,(#24216,#24217,#24218,#24219,#24220,
#24221,#24222,#24223,#24224,#24225,#24226,#24227,#24228,#24229,#24230,#24231,
#24232,#24233,#24234,#24235,#24236,#24237,#24238,#24239,#24240,#24241,#24242,
#24243,#24244,#24245,#24246,#24247,#24248,#24249,#24250,#24251,#24252,#24253,
#24254,#24255,#24256,#24257,#24258),.UNSPECIFIED.,.F.,.F.,(4,3,3,3,3,3,
3,3,3,3,3,3,3,3,4),(31.8589872064524,31.9794602741135,32.4791393408966,
32.9788184076796,33.4784974744626,33.9781765412456,34.4778556080286,34.9775346748117,
35.4772137415947,35.9768928083777,36.4765718751607,36.9762509419437,37.4759300087267,
37.9756090755098,38.142172513632),.UNSPECIFIED.);
#492=B_SPLINE_CURVE_WITH_KNOTS('',3,(#24263,#24264,#24265,#24266,#24267,
#24268,#24269,#24270,#24271,#24272,#24273,#24274,#24275,#24276,#24277,#24278,
#24279,#24280,#24281,#24282,#24283,#24284,#24285,#24286,#24287,#24288,#24289,
#24290,#24291,#24292,#24293,#24294,#24295,#24296,#24297,#24298,#24299,#24300,
#24301,#24302,#24303,#24304,#24305),.UNSPECIFIED.,.F.,.F.,(4,3,3,3,3,3,
3,3,3,3,3,3,3,3,4),(-47.6810126419616,-47.4695113443872,-46.9698322776042,
-46.4701532108212,-45.9704741440381,-45.4707950772551,-44.9711160104721,
-44.4714369436891,-43.971757876906,-43.472078810123,-42.97239974334,-42.472720676557,
-41.973041609774,-41.4733625429909,-41.397827334782),.UNSPECIFIED.);
#493=B_SPLINE_CURVE_WITH_KNOTS('',3,(#24306,#24307,#24308,#24309,#24310,
#24311,#24312,#24313,#24314,#24315,#24316,#24317,#24318,#24319,#24320,#24321,
#24322,#24323,#24324,#24325,#24326,#24327,#24328,#24329,#24330,#24331,#24332,
#24333,#24334,#24335,#24336,#24337,#24338,#24339,#24340,#24341,#24342,#24343,
#24344,#24345),.UNSPECIFIED.,.F.,.F.,(4,3,3,3,3,3,3,3,3,3,3,3,3,4),(38.142172513632,
38.4752881422928,38.9749672090758,39.4746462758589,39.9743253426419,40.4740044094249,
40.973683476208,41.473362542991,41.973041609774,42.472720676557,42.9723997433401,
43.4720788101231,43.9717578769061,44.4253578208116),.UNSPECIFIED.);
#494=B_SPLINE_CURVE_WITH_KNOTS('',3,(#24350,#24351,#24352,#24353,#24354,
#24355,#24356,#24357,#24358,#24359,#24360,#24361,#24362,#24363,#24364,#24365,
#24366,#24367,#24368,#24369,#24370,#24371,#24372,#24373,#24374,#24375,#24376,
#24377),.UNSPECIFIED.,.F.,.F.,(4,3,3,3,3,3,3,3,3,4),(-53.9641979491412,
-52.9659810790005,-51.9666229454344,-50.9672648118684,-49.9679066783023,
-49.4682276115193,-48.9685485447363,-48.4688694779533,-47.9691904111702,
-47.6810126419616),.UNSPECIFIED.);
#495=B_SPLINE_CURVE_WITH_KNOTS('',3,(#24378,#24379,#24380,#24381,#24382,
#24383,#24384,#24385,#24386,#24387,#24388,#24389,#24390,#24391,#24392,#24393,
#24394,#24395,#24396,#24397,#24398,#24399,#24400,#24401,#24402,#24403,#24404,
#24405,#24406,#24407,#24408,#24409,#24410,#24411,#24412,#24413,#24414,#24415,
#24416,#24417),.UNSPECIFIED.,.F.,.F.,(4,3,3,3,3,3,3,3,3,3,3,3,3,4),(44.4253578208116,
44.4714369436892,44.9711160104722,45.4707950772552,45.9704741440382,46.4701532108212,
46.9698322776042,47.4695113443873,47.9691904111703,48.4688694779533,48.9685485447363,
49.4682276115193,49.9679066783024,50.7085431279912),.UNSPECIFIED.);
#496=B_SPLINE_CURVE_WITH_KNOTS('',3,(#24422,#24423,#24424,#24425,#24426,
#24427,#24428,#24429,#24430,#24431,#24432,#24433,#24434,#24435,#24436,#24437,
#24438,#24439,#24440,#24441,#24442,#24443),.UNSPECIFIED.,.F.,.F.,(4,3,3,
3,3,3,3,4),(-60.2473832563207,-59.9614880139628,-58.9621298803968,-57.9627717468307,
-56.9634136132647,-55.9640554796986,-54.9646973461326,-53.9641979491412),
 .UNSPECIFIED.);
#497=B_SPLINE_CURVE_WITH_KNOTS('',3,(#24444,#24445,#24446,#24447,#24448,
#24449,#24450,#24451,#24452,#24453,#24454,#24455,#24456,#24457,#24458,#24459,
#24460,#24461,#24462,#24463,#24464,#24465,#24466,#24467,#24468),
 .UNSPECIFIED.,.F.,.F.,(4,3,3,3,3,3,3,3,4),(50.7085431279912,50.9672648118684,
51.9666229454345,52.9659810790005,53.9653392125666,54.9646973461326,55.9640554796987,
56.9634136132647,56.9917284351708),.UNSPECIFIED.);
#498=B_SPLINE_CURVE_WITH_KNOTS('',3,(#24473,#24474,#24475,#24476,#24477,
#24478,#24479,#24480,#24481,#24482,#24483,#24484,#24485,#24486,#24487,#24488,
#24489,#24490,#24491,#24492,#24493,#24494),.UNSPECIFIED.,.F.,.F.,(4,3,3,
3,3,3,3,4),(-66.5305685635003,-65.9576368153591,-64.958278681793,-63.958920548227,
-62.9595624146609,-61.9602042810949,-60.9608461475288,-60.2473832563207),
 .UNSPECIFIED.);
#499=B_SPLINE_CURVE_WITH_KNOTS('',3,(#24495,#24496,#24497,#24498,#24499,
#24500,#24501,#24502,#24503,#24504,#24505,#24506,#24507,#24508,#24509,#24510,
#24511,#24512,#24513,#24514,#24515,#24516),.UNSPECIFIED.,.F.,.F.,(4,3,3,
3,3,3,3,4),(56.9917284351708,57.9627717468308,58.9621298803968,59.9614880139629,
60.9608461475289,61.960204281095,62.959562414661,63.2749137423504),
 .UNSPECIFIED.);
#500=B_SPLINE_CURVE_WITH_KNOTS('',3,(#24521,#24522,#24523,#24524,#24525,
#24526,#24527,#24528,#24529,#24530,#24531,#24532,#24533,#24534,#24535,#24536,
#24537,#24538,#24539,#24540,#24541,#24542),.UNSPECIFIED.,.F.,.F.,(4,3,3,
3,3,3,3,4),(-72.8137538706799,-71.9537856167554,-70.9544274831893,-69.9550693496233,
-68.9557112160572,-67.9563530824912,-66.9569949489251,-66.5305685635003),
 .UNSPECIFIED.);
#501=B_SPLINE_CURVE_WITH_KNOTS('',3,(#24543,#24544,#24545,#24546,#24547,
#24548,#24549,#24550,#24551,#24552,#24553,#24554,#24555,#24556,#24557,#24558,
#24559,#24560,#24561,#24562,#24563,#24564),.UNSPECIFIED.,.F.,.F.,(4,3,3,
3,3,3,3,4),(63.2749137423504,63.958920548227,64.9582786817931,65.9576368153591,
66.9569949489252,67.9563530824912,68.9557112160573,69.55809904953),
 .UNSPECIFIED.);
#502=B_SPLINE_CURVE_WITH_KNOTS('',3,(#24569,#24570,#24571,#24572,#24573,
#24574,#24575,#24576,#24577,#24578,#24579,#24580,#24581,#24582,#24583,#24584,
#24585,#24586,#24587,#24588,#24589,#24590,#24591,#24592,#24593),
 .UNSPECIFIED.,.F.,.F.,(4,3,3,3,3,3,3,3,4),(-79.0969391778595,-78.9492925517177,
-77.9499344181516,-76.9505762845856,-75.9512181510195,-74.9518600174535,
-73.9525018838875,-72.9531437503214,-72.8137538706799),.UNSPECIFIED.);
#503=B_SPLINE_CURVE_WITH_KNOTS('',3,(#24594,#24595,#24596,#24597,#24598,
#24599,#24600,#24601,#24602,#24603,#24604,#24605,#24606,#24607,#24608,#24609,
#24610,#24611,#24612,#24613,#24614,#24615),.UNSPECIFIED.,.F.,.F.,(4,3,3,
3,3,3,3,4),(69.55809904953,69.9550693496233,70.9544274831893,71.9537856167554,
72.9531437503215,73.9525018838875,74.9518600174536,75.8412843567096),
 .UNSPECIFIED.);
#504=B_SPLINE_CURVE_WITH_KNOTS('',3,(#24620,#24621,#24622,#24623,#24624,
#24625,#24626,#24627,#24628,#24629,#24630,#24631,#24632,#24633,#24634,#24635,
#24636,#24637,#24638,#24639,#24640,#24641),.UNSPECIFIED.,.F.,.F.,(4,3,3,
3,3,3,3,4),(-85.3801244850391,-84.945441353114,-83.9460832195479,-82.9467250859819,
-81.9473669524158,-80.9480088188498,-79.9486506852837,-79.0969391778595),
 .UNSPECIFIED.);
#505=B_SPLINE_CURVE_WITH_KNOTS('',3,(#24642,#24643,#24644,#24645,#24646,
#24647,#24648,#24649,#24650,#24651,#24652,#24653,#24654,#24655,#24656,#24657,
#24658,#24659,#24660,#24661,#24662,#24663,#24664,#24665,#24666),
 .UNSPECIFIED.,.F.,.F.,(4,3,3,3,3,3,3,3,4),(75.8412843567096,75.9512181510196,
76.9505762845857,77.9499344181517,78.9492925517178,79.9486506852838,80.9480088188499,
81.9473669524159,82.1244696638892),.UNSPECIFIED.);
#506=B_SPLINE_CURVE_WITH_KNOTS('',3,(#24671,#24672,#24673,#24674,#24675,
#24676,#24677,#24678,#24679,#24680,#24681,#24682,#24683,#24684,#24685,#24686,
#24687,#24688,#24689,#24690,#24691,#24692),.UNSPECIFIED.,.F.,.F.,(4,3,3,
3,3,3,3,4),(-91.6633097922187,-90.9415901545102,-89.9422320209442,-88.9428738873782,
-87.9435157538121,-86.944157620246,-85.94479948668,-85.3801244850391),
 .UNSPECIFIED.);
#507=B_SPLINE_CURVE_WITH_KNOTS('',3,(#24693,#24694,#24695,#24696,#24697,
#24698,#24699,#24700,#24701,#24702,#24703,#24704,#24705,#24706,#24707,#24708,
#24709,#24710,#24711,#24712,#24713,#24714),.UNSPECIFIED.,.F.,.F.,(4,3,3,
3,3,3,3,4),(82.1244696638892,82.946725085982,83.946083219548,84.9454413531141,
85.9447994866801,86.9441576202461,87.9435157538122,88.4076549710687),
 .UNSPECIFIED.);
#508=B_SPLINE_CURVE_WITH_KNOTS('',3,(#24719,#24720,#24721,#24722,#24723,
#24724,#24725,#24726,#24727,#24728,#24729,#24730,#24731,#24732,#24733,#24734,
#24735,#24736,#24737,#24738,#24739,#24740,#24741,#24742,#24743),
 .UNSPECIFIED.,.F.,.F.,(4,3,3,3,3,3,3,3,4),(-97.9464950993983,-97.9370970894726,
-96.9377389559065,-95.9383808223405,-94.9390226887744,-93.9396645552084,
-92.9403064216423,-91.9409482880763,-91.6633097922187),.UNSPECIFIED.);
#509=B_SPLINE_CURVE_WITH_KNOTS('',3,(#24744,#24745,#24746,#24747,#24748,
#24749,#24750,#24751,#24752,#24753,#24754,#24755,#24756,#24757,#24758,#24759,
#24760,#24761,#24762,#24763,#24764,#24765),.UNSPECIFIED.,.F.,.F.,(4,3,3,
3,3,3,3,4),(88.4076549710687,88.9428738873782,89.9422320209442,90.9415901545103,
91.9409482880763,92.9403064216424,93.9396645552084,94.6908402782483),
 .UNSPECIFIED.);
#510=B_SPLINE_CURVE_WITH_KNOTS('',3,(#24770,#24771,#24772,#24773,#24774,
#24775,#24776,#24777,#24778,#24779,#24780,#24781,#24782,#24783,#24784,#24785,
#24786,#24787,#24788,#24789,#24790,#24791),.UNSPECIFIED.,.F.,.F.,(4,3,3,
3,3,3,3,4),(-104.229680406578,-103.933245890869,-102.933887757303,-101.934529623737,
-100.935171490171,-99.9358133566047,-98.9364552230386,-97.9464950993983),
 .UNSPECIFIED.);
#511=B_SPLINE_CURVE_WITH_KNOTS('',3,(#24792,#24793,#24794,#24795,#24796,
#24797,#24798,#24799,#24800,#24801,#24802,#24803,#24804,#24805,#24806,#24807,
#24808,#24809,#24810,#24811,#24812,#24813,#24814,#24815,#24816),
 .UNSPECIFIED.,.F.,.F.,(4,3,3,3,3,3,3,3,4),(94.6908402782483,94.9390226887745,
95.9383808223405,96.9377389559065,97.9370970894726,98.9364552230386,99.9358133566047,
100.935171490171,100.974025585428),.UNSPECIFIED.);
#512=B_SPLINE_CURVE_WITH_KNOTS('',3,(#24821,#24822,#24823,#24824,#24825,
#24826,#24827,#24828,#24829,#24830,#24831,#24832,#24833,#24834,#24835,#24836,
#24837,#24838,#24839,#24840,#24841,#24842),.UNSPECIFIED.,.F.,.F.,(4,3,3,
3,3,3,3,4),(-110.512865713757,-109.929394692265,-108.930036558699,-107.930678425133,
-106.931320291567,-105.931962158001,-104.932604024435,-104.229680406578),
 .UNSPECIFIED.);
#513=B_SPLINE_CURVE_WITH_KNOTS('',3,(#24843,#24844,#24845,#24846,#24847,
#24848,#24849,#24850,#24851,#24852,#24853,#24854,#24855,#24856,#24857,#24858,
#24859,#24860,#24861,#24862,#24863,#24864),.UNSPECIFIED.,.F.,.F.,(4,3,3,
3,3,3,3,4),(100.974025585428,101.934529623737,102.933887757303,103.933245890869,
104.932604024435,105.931962158001,106.931320291567,107.257210892608),
 .UNSPECIFIED.);
#514=B_SPLINE_CURVE_WITH_KNOTS('',3,(#24869,#24870,#24871,#24872,#24873,
#24874,#24875,#24876,#24877,#24878,#24879,#24880,#24881,#24882,#24883,#24884,
#24885,#24886,#24887,#24888,#24889,#24890),.UNSPECIFIED.,.F.,.F.,(4,3,3,
3,3,3,3,4),(-116.796051020937,-115.925543493661,-114.926185360095,-113.926827226529,
-112.927469092963,-111.928110959397,-110.928752825831,-110.512865713757),
 .UNSPECIFIED.);
#515=B_SPLINE_CURVE_WITH_KNOTS('',3,(#24891,#24892,#24893,#24894,#24895,
#24896,#24897,#24898,#24899,#24900,#24901,#24902,#24903,#24904,#24905,#24906,
#24907,#24908,#24909,#24910,#24911,#24912),.UNSPECIFIED.,.F.,.F.,(4,3,3,
3,3,3,3,4),(107.257210892608,107.930678425133,108.930036558699,109.929394692265,
110.928752825831,111.928110959397,112.927469092963,113.540396199787),
 .UNSPECIFIED.);
#516=B_SPLINE_CURVE_WITH_KNOTS('',3,(#24917,#24918,#24919,#24920,#24921,
#24922,#24923,#24924,#24925,#24926,#24927,#24928,#24929,#24930,#24931,#24932,
#24933,#24934,#24935,#24936,#24937,#24938,#24939,#24940,#24941),
 .UNSPECIFIED.,.F.,.F.,(4,3,3,3,3,3,3,3,4),(-123.079236328117,-122.921050428624,
-121.921692295058,-120.922334161492,-119.922976027926,-118.92361789436,
-117.924259760793,-116.924901627227,-116.796051020937),.UNSPECIFIED.);
#517=B_SPLINE_CURVE_WITH_KNOTS('',3,(#24942,#24943,#24944,#24945,#24946,
#24947,#24948,#24949,#24950,#24951,#24952,#24953,#24954,#24955,#24956,#24957,
#24958,#24959,#24960,#24961,#24962,#24963),.UNSPECIFIED.,.F.,.F.,(4,3,3,
3,3,3,3,4),(113.540396199787,113.926827226529,114.926185360095,115.925543493661,
116.924901627228,117.924259760794,118.92361789436,119.823581506967),
 .UNSPECIFIED.);
#518=B_SPLINE_CURVE_WITH_KNOTS('',3,(#24968,#24969,#24970,#24971,#24972,
#24973,#24974,#24975,#24976,#24977,#24978,#24979,#24980,#24981,#24982,#24983,
#24984,#24985,#24986,#24987,#24988,#24989),.UNSPECIFIED.,.F.,.F.,(4,3,3,
3,3,3,3,4),(-129.362421635296,-128.91719923002,-127.917841096454,-126.918482962888,
-125.919124829322,-124.919766695756,-123.92040856219,-123.079236328117),
 .UNSPECIFIED.);
#519=B_SPLINE_CURVE_WITH_KNOTS('',3,(#24990,#24991,#24992,#24993,#24994,
#24995,#24996,#24997,#24998,#24999,#25000,#25001,#25002,#25003,#25004,#25005,
#25006,#25007,#25008,#25009,#25010,#25011,#25012,#25013,#25014),
 .UNSPECIFIED.,.F.,.F.,(4,3,3,3,3,3,3,3,4),(119.823581506967,119.922976027926,
120.922334161492,121.921692295058,122.921050428624,123.92040856219,124.919766695756,
125.919124829322,126.106766814146),.UNSPECIFIED.);
#520=B_SPLINE_CURVE_WITH_KNOTS('',3,(#25019,#25020,#25021,#25022,#25023,
#25024,#25025,#25026,#25027,#25028,#25029,#25030,#25031,#25032,#25033,#25034,
#25035,#25036,#25037,#25038,#25039,#25040),.UNSPECIFIED.,.F.,.F.,(4,3,3,
3,3,3,3,4),(-135.645606942476,-134.913348031416,-133.91398989785,-132.914631764284,
-131.915273630718,-130.915915497152,-129.916557363586,-129.362421635296),
 .UNSPECIFIED.);
#521=B_SPLINE_CURVE_WITH_KNOTS('',3,(#25041,#25042,#25043,#25044,#25045,
#25046,#25047,#25048,#25049,#25050,#25051,#25052,#25053,#25054,#25055,#25056,
#25057,#25058,#25059,#25060,#25061,#25062),.UNSPECIFIED.,.F.,.F.,(4,3,3,
3,3,3,3,4),(126.106766814146,126.918482962888,127.917841096454,128.91719923002,
129.916557363586,130.915915497152,131.915273630718,132.389952121326),
 .UNSPECIFIED.);
#522=B_SPLINE_CURVE_WITH_KNOTS('',3,(#25067,#25068,#25069,#25070,#25071,
#25072,#25073,#25074,#25075,#25076,#25077,#25078,#25079,#25080,#25081,#25082,
#25083,#25084,#25085,#25086,#25087,#25088,#25089,#25090,#25091),
 .UNSPECIFIED.,.F.,.F.,(4,3,3,3,3,3,3,3,4),(-141.928792249655,-141.908854966379,
-140.909496832813,-139.910138699247,-138.91078056568,-137.911422432114,
-136.912064298548,-135.912706164982,-135.645606942476),.UNSPECIFIED.);
#523=B_SPLINE_CURVE_WITH_KNOTS('',3,(#25092,#25093,#25094,#25095,#25096,
#25097,#25098,#25099,#25100,#25101,#25102,#25103,#25104,#25105,#25106,#25107,
#25108,#25109,#25110,#25111,#25112,#25113),.UNSPECIFIED.,.F.,.F.,(4,3,3,
3,3,3,3,4),(132.389952121326,132.914631764284,133.91398989785,134.913348031416,
135.912706164982,136.912064298549,137.911422432115,138.673137428505),
 .UNSPECIFIED.);
#524=B_SPLINE_CURVE_WITH_KNOTS('',3,(#25118,#25119,#25120,#25121,#25122,
#25123,#25124,#25125,#25126,#25127,#25128,#25129,#25130,#25131,#25132,#25133,
#25134,#25135,#25136,#25137,#25138,#25139),.UNSPECIFIED.,.F.,.F.,(4,3,3,
3,3,3,3,4),(-148.211977556835,-147.905003767775,-146.905645634209,-145.906287500643,
-144.906929367077,-143.907571233511,-142.908213099945,-141.928792249655),
 .UNSPECIFIED.);
#525=B_SPLINE_CURVE_WITH_KNOTS('',3,(#25140,#25141,#25142,#25143,#25144,
#25145,#25146,#25147,#25148,#25149,#25150,#25151,#25152,#25153,#25154,#25155,
#25156,#25157,#25158,#25159,#25160,#25161,#25162,#25163,#25164),
 .UNSPECIFIED.,.F.,.F.,(4,3,3,3,3,3,3,3,4),(138.673137428505,138.910780565681,
139.910138699247,140.909496832813,141.908854966379,142.908213099945,143.907571233511,
144.906929367077,144.956322735685),.UNSPECIFIED.);
#526=B_SPLINE_CURVE_WITH_KNOTS('',3,(#25169,#25170,#25171,#25172,#25173,
#25174,#25175,#25176,#25177,#25178,#25179,#25180,#25181,#25182,#25183,#25184,
#25185,#25186,#25187,#25188,#25189,#25190),.UNSPECIFIED.,.F.,.F.,(4,3,3,
3,3,3,3,4),(-154.495162864015,-153.901152569171,-152.901794435605,-151.902436302039,
-150.903078168473,-149.903720034907,-148.904361901341,-148.211977556835),
 .UNSPECIFIED.);
#527=B_SPLINE_CURVE_WITH_KNOTS('',3,(#25191,#25192,#25193,#25194,#25195,
#25196,#25197,#25198,#25199,#25200,#25201,#25202,#25203,#25204,#25205,#25206,
#25207,#25208,#25209,#25210,#25211,#25212),.UNSPECIFIED.,.F.,.F.,(4,3,3,
3,3,3,3,4),(144.956322735685,145.906287500643,146.905645634209,147.905003767775,
148.904361901341,149.903720034907,150.903078168473,151.239508042865),
 .UNSPECIFIED.);
#528=B_SPLINE_CURVE_WITH_KNOTS('',3,(#25217,#25218,#25219,#25220,#25221,
#25222,#25223,#25224,#25225,#25226,#25227,#25228,#25229,#25230,#25231,#25232,
#25233,#25234,#25235,#25236,#25237,#25238),.UNSPECIFIED.,.F.,.F.,(4,3,3,
3,3,3,3,4),(-160.778348171194,-159.897301370567,-158.897943237001,-157.898585103435,
-156.899226969869,-155.899868836303,-154.900510702737,-154.495162864015),
 .UNSPECIFIED.);
#529=B_SPLINE_CURVE_WITH_KNOTS('',3,(#25239,#25240,#25241,#25242,#25243,
#25244,#25245,#25246,#25247,#25248,#25249,#25250,#25251,#25252,#25253,#25254,
#25255,#25256,#25257,#25258,#25259,#25260),.UNSPECIFIED.,.F.,.F.,(4,3,3,
3,3,3,3,4),(151.239508042865,151.902436302039,152.901794435605,153.901152569171,
154.900510702737,155.899868836303,156.899226969869,157.522693350044),
 .UNSPECIFIED.);
#530=B_SPLINE_CURVE_WITH_KNOTS('',3,(#25265,#25266,#25267,#25268,#25269,
#25270,#25271,#25272,#25273,#25274,#25275,#25276,#25277,#25278,#25279,#25280,
#25281,#25282,#25283,#25284,#25285,#25286,#25287,#25288,#25289),
 .UNSPECIFIED.,.F.,.F.,(4,3,3,3,3,3,3,3,4),(-167.061533478374,-166.89280830553,
-165.893450171964,-164.894092038398,-163.894733904832,-162.895375771266,
-161.8960176377,-160.896659504134,-160.778348171194),.UNSPECIFIED.);
#531=B_SPLINE_CURVE_WITH_KNOTS('',3,(#25290,#25291,#25292,#25293,#25294,
#25295,#25296,#25297,#25298,#25299,#25300,#25301,#25302,#25303,#25304,#25305,
#25306,#25307,#25308,#25309,#25310,#25311),.UNSPECIFIED.,.F.,.F.,(4,3,3,
3,3,3,3,4),(157.522693350044,157.898585103435,158.897943237002,159.897301370568,
160.896659504134,161.8960176377,162.895375771266,163.805878657224),
 .UNSPECIFIED.);
#532=B_SPLINE_CURVE_WITH_KNOTS('',3,(#25316,#25317,#25318,#25319,#25320,
#25321,#25322,#25323,#25324,#25325,#25326,#25327,#25328,#25329,#25330,#25331,
#25332,#25333,#25334,#25335,#25336,#25337),.UNSPECIFIED.,.F.,.F.,(4,3,3,
3,3,3,3,4),(-173.344718785553,-172.888957106926,-171.88959897336,-170.890240839794,
-169.890882706228,-168.891524572662,-167.892166439096,-167.061533478374),
 .UNSPECIFIED.);
#533=B_SPLINE_CURVE_WITH_KNOTS('',3,(#25338,#25339,#25340,#25341,#25342,
#25343,#25344,#25345,#25346,#25347,#25348,#25349,#25350,#25351,#25352,#25353,
#25354,#25355,#25356,#25357,#25358,#25359,#25360,#25361,#25362),
 .UNSPECIFIED.,.F.,.F.,(4,3,3,3,3,3,3,3,4),(163.805878657224,163.894733904832,
164.894092038398,165.893450171964,166.89280830553,167.892166439096,168.891524572662,
169.890882706228,170.089063964403),.UNSPECIFIED.);
#534=B_SPLINE_CURVE_WITH_KNOTS('',3,(#25367,#25368,#25369,#25370,#25371,
#25372,#25373,#25374,#25375,#25376,#25377,#25378,#25379,#25380,#25381,#25382,
#25383,#25384,#25385,#25386,#25387,#25388),.UNSPECIFIED.,.F.,.F.,(4,3,3,
3,3,3,3,4),(-179.627904092733,-178.885105908322,-177.885747774756,-176.88638964119,
-175.887031507624,-174.887673374058,-173.888315240492,-173.344718785553),
 .UNSPECIFIED.);
#535=B_SPLINE_CURVE_WITH_KNOTS('',3,(#25389,#25390,#25391,#25392,#25393,
#25394,#25395,#25396,#25397,#25398,#25399,#25400,#25401,#25402,#25403,#25404,
#25405,#25406,#25407,#25408,#25409,#25410),.UNSPECIFIED.,.F.,.F.,(4,3,3,
3,3,3,3,4),(170.089063964403,170.890240839794,171.88959897336,172.888957106926,
173.888315240492,174.887673374058,175.887031507624,176.372249271583),
 .UNSPECIFIED.);
#536=B_SPLINE_CURVE_WITH_KNOTS('',3,(#25415,#25416,#25417,#25418,#25419,
#25420,#25421,#25422,#25423,#25424,#25425,#25426,#25427,#25428,#25429,#25430,
#25431,#25432,#25433,#25434,#25435,#25436,#25437,#25438,#25439),
 .UNSPECIFIED.,.F.,.F.,(4,3,3,3,3,3,3,3,4),(-185.911089399912,-185.880612843285,
-184.881254709719,-183.881896576153,-182.882538442587,-181.88318030902,
-180.883822175454,-179.884464041888,-179.627904092733),.UNSPECIFIED.);
#537=B_SPLINE_CURVE_WITH_KNOTS('',3,(#25440,#25441,#25442,#25443,#25444,
#25445,#25446,#25447,#25448,#25449,#25450,#25451,#25452,#25453,#25454,#25455,
#25456,#25457,#25458,#25459,#25460,#25461),.UNSPECIFIED.,.F.,.F.,(4,3,3,
3,3,3,3,4),(176.372249271583,176.88638964119,177.885747774756,178.885105908322,
179.884464041889,180.883822175455,181.883180309021,182.655434578762),
 .UNSPECIFIED.);
#538=B_SPLINE_CURVE_WITH_KNOTS('',3,(#25466,#25467,#25468,#25469,#25470,
#25471,#25472,#25473,#25474,#25475,#25476,#25477,#25478,#25479,#25480,#25481,
#25482,#25483,#25484,#25485,#25486,#25487),.UNSPECIFIED.,.F.,.F.,(4,3,3,
3,3,3,3,4),(-192.194274707092,-191.876761644681,-190.877403511115,-189.878045377549,
-188.878687243983,-187.879329110417,-186.879970976851,-185.911089399912),
 .UNSPECIFIED.);
#539=B_SPLINE_CURVE_WITH_KNOTS('',3,(#25488,#25489,#25490,#25491,#25492,
#25493,#25494,#25495,#25496,#25497,#25498,#25499,#25500,#25501,#25502,#25503,
#25504,#25505,#25506,#25507,#25508,#25509,#25510,#25511,#25512),
 .UNSPECIFIED.,.F.,.F.,(4,3,3,3,3,3,3,3,4),(182.655434578762,182.882538442587,
183.881896576153,184.881254709719,185.880612843285,186.879970976851,187.879329110417,
188.878687243983,188.938619885942),.UNSPECIFIED.);
#540=B_SPLINE_CURVE_WITH_KNOTS('',3,(#25517,#25518,#25519,#25520,#25521,
#25522,#25523,#25524,#25525,#25526,#25527,#25528,#25529,#25530,#25531,#25532,
#25533,#25534,#25535,#25536,#25537,#25538),.UNSPECIFIED.,.F.,.F.,(4,3,3,
3,3,3,3,4),(-198.477460014271,-197.872910446077,-196.873552312511,-195.874194178945,
-194.874836045379,-193.875477911813,-192.876119778247,-192.194274707092),
 .UNSPECIFIED.);
#541=B_SPLINE_CURVE_WITH_KNOTS('',3,(#25539,#25540,#25541,#25542,#25543,
#25544,#25545,#25546,#25547,#25548,#25549,#25550,#25551,#25552,#25553,#25554,
#25555,#25556,#25557,#25558,#25559,#25560),.UNSPECIFIED.,.F.,.F.,(4,3,3,
3,3,3,3,4),(188.938619885942,189.878045377549,190.877403511115,191.876761644681,
192.876119778247,193.875477911813,194.874836045379,195.221805193122),
 .UNSPECIFIED.);
#542=B_SPLINE_CURVE_WITH_KNOTS('',3,(#25565,#25566,#25567,#25568,#25569,
#25570,#25571,#25572,#25573,#25574,#25575,#25576,#25577,#25578,#25579,#25580,
#25581,#25582,#25583,#25584,#25585,#25586),.UNSPECIFIED.,.F.,.F.,(4,3,3,
3,3,3,3,4),(-204.760645321451,-203.869059247473,-202.869701113907,-201.870342980341,
-200.870984846775,-199.871626713209,-198.872268579643,-198.477460014271),
 .UNSPECIFIED.);
#543=B_SPLINE_CURVE_WITH_KNOTS('',3,(#25587,#25588,#25589,#25590,#25591,
#25592,#25593,#25594,#25595,#25596,#25597,#25598,#25599,#25600,#25601,#25602,
#25603,#25604,#25605,#25606,#25607,#25608),.UNSPECIFIED.,.F.,.F.,(4,3,3,
3,3,3,3,4),(195.221805193122,195.874194178945,196.873552312511,197.872910446077,
198.872268579643,199.871626713209,200.870984846776,201.504990500301),
 .UNSPECIFIED.);
#544=B_SPLINE_CURVE_WITH_KNOTS('',3,(#25613,#25614,#25615,#25616,#25617,
#25618,#25619,#25620,#25621,#25622,#25623,#25624,#25625,#25626,#25627,#25628,
#25629,#25630,#25631,#25632,#25633,#25634,#25635,#25636,#25637),
 .UNSPECIFIED.,.F.,.F.,(4,3,3,3,3,3,3,3,4),(-211.043830628631,-210.864566182436,
-209.86520804887,-208.865849915304,-207.866491781738,-206.867133648172,
-205.867775514606,-204.86841738104,-204.760645321451),.UNSPECIFIED.);
#545=B_SPLINE_CURVE_WITH_KNOTS('',3,(#25638,#25639,#25640,#25641,#25642,
#25643,#25644,#25645,#25646,#25647,#25648,#25649,#25650,#25651,#25652,#25653,
#25654,#25655,#25656,#25657,#25658,#25659),.UNSPECIFIED.,.F.,.F.,(4,3,3,
3,3,3,3,4),(201.504990500301,201.870342980342,202.869701113908,203.869059247474,
204.86841738104,205.867775514606,206.867133648172,207.788175807481),
 .UNSPECIFIED.);
#546=B_SPLINE_CURVE_WITH_KNOTS('',3,(#25664,#25665,#25666,#25667,#25668,
#25669,#25670,#25671,#25672,#25673,#25674,#25675,#25676,#25677,#25678,#25679,
#25680,#25681,#25682,#25683,#25684,#25685),.UNSPECIFIED.,.F.,.F.,(4,3,3,
3,3,3,3,4),(-217.32701593581,-216.860714983832,-215.861356850266,-214.8619987167,
-213.862640583134,-212.863282449568,-211.863924316002,-211.043830628631),
 .UNSPECIFIED.);
#547=B_SPLINE_CURVE_WITH_KNOTS('',3,(#25686,#25687,#25688,#25689,#25690,
#25691,#25692,#25693,#25694,#25695,#25696,#25697,#25698,#25699,#25700,#25701,
#25702,#25703,#25704,#25705,#25706,#25707,#25708,#25709,#25710),
 .UNSPECIFIED.,.F.,.F.,(4,3,3,3,3,3,3,3,4),(207.788175807481,207.866491781738,
208.865849915304,209.86520804887,210.864566182436,211.863924316002,212.863282449568,
213.862640583134,214.07136111466),.UNSPECIFIED.);
#548=B_SPLINE_CURVE_WITH_KNOTS('',3,(#25715,#25716,#25717,#25718,#25719,
#25720,#25721,#25722,#25723,#25724,#25725,#25726,#25727,#25728,#25729,#25730,
#25731,#25732,#25733,#25734,#25735,#25736),.UNSPECIFIED.,.F.,.F.,(4,3,3,
3,3,3,3,4),(-223.61020124299,-222.856863785228,-221.857505651662,-220.858147518096,
-219.85878938453,-218.859431250964,-217.860073117398,-217.32701593581),
 .UNSPECIFIED.);
#549=B_SPLINE_CURVE_WITH_KNOTS('',3,(#25737,#25738,#25739,#25740,#25741,
#25742,#25743,#25744,#25745,#25746,#25747,#25748,#25749,#25750,#25751,#25752,
#25753,#25754,#25755,#25756,#25757,#25758),.UNSPECIFIED.,.F.,.F.,(4,3,3,
3,3,3,3,4),(214.07136111466,214.8619987167,215.861356850266,216.860714983832,
217.860073117398,218.859431250964,219.85878938453,220.35454642184),
 .UNSPECIFIED.);
#550=B_SPLINE_CURVE_WITH_KNOTS('',3,(#25763,#25764,#25765,#25766,#25767,
#25768,#25769,#25770,#25771,#25772,#25773,#25774,#25775,#25776,#25777,#25778,
#25779,#25780,#25781,#25782,#25783,#25784,#25785,#25786,#25787),
 .UNSPECIFIED.,.F.,.F.,(4,3,3,3,3,3,3,3,4),(-229.893386550169,-229.852370720191,
-228.853012586625,-227.853654453059,-226.854296319493,-225.854938185927,
-224.85558005236,-223.856221918794,-223.61020124299),.UNSPECIFIED.);
#551=B_SPLINE_CURVE_WITH_KNOTS('',3,(#25788,#25789,#25790,#25791,#25792,
#25793,#25794,#25795,#25796,#25797,#25798,#25799,#25800,#25801,#25802,#25803,
#25804,#25805,#25806,#25807,#25808,#25809),.UNSPECIFIED.,.F.,.F.,(4,3,3,
3,3,3,3,4),(220.35454642184,220.858147518096,221.857505651663,222.856863785229,
223.856221918795,224.855580052361,225.854938185927,226.637731729019),
 .UNSPECIFIED.);
#552=B_SPLINE_CURVE_WITH_KNOTS('',3,(#25814,#25815,#25816,#25817,#25818,
#25819,#25820,#25821,#25822,#25823,#25824,#25825,#25826,#25827,#25828,#25829,
#25830,#25831,#25832,#25833,#25834,#25835),.UNSPECIFIED.,.F.,.F.,(4,3,3,
3,3,3,3,4),(-236.176571857349,-235.848519521587,-234.849161388021,-233.849803254455,
-232.850445120889,-231.851086987323,-230.851728853757,-229.893386550169),
 .UNSPECIFIED.);
#553=B_SPLINE_CURVE_WITH_KNOTS('',3,(#25836,#25837,#25838,#25839,#25840,
#25841,#25842,#25843,#25844,#25845,#25846,#25847,#25848,#25849,#25850,#25851,
#25852,#25853,#25854,#25855,#25856,#25857,#25858,#25859,#25860),
 .UNSPECIFIED.,.F.,.F.,(4,3,3,3,3,3,3,3,4),(226.637731729019,226.854296319493,
227.853654453059,228.853012586625,229.852370720191,230.851728853757,231.851086987323,
232.850445120889,232.920917036199),.UNSPECIFIED.);
#554=B_SPLINE_CURVE_WITH_KNOTS('',3,(#25865,#25866,#25867,#25868,#25869,
#25870,#25871,#25872,#25873,#25874,#25875,#25876,#25877,#25878,#25879,#25880,
#25881,#25882,#25883,#25884,#25885,#25886),.UNSPECIFIED.,.F.,.F.,(4,3,3,
3,3,3,3,4),(-242.459757164528,-241.844668322983,-240.845310189417,-239.845952055851,
-238.846593922285,-237.847235788719,-236.847877655153,-236.176571857349),
 .UNSPECIFIED.);
#555=B_SPLINE_CURVE_WITH_KNOTS('',3,(#25887,#25888,#25889,#25890,#25891,
#25892,#25893,#25894,#25895,#25896,#25897,#25898,#25899,#25900,#25901,#25902,
#25903,#25904,#25905,#25906,#25907,#25908),.UNSPECIFIED.,.F.,.F.,(4,3,3,
3,3,3,3,4),(232.920917036199,233.849803254455,234.849161388021,235.848519521587,
236.847877655153,237.847235788719,238.846593922285,239.204102343378),
 .UNSPECIFIED.);
#556=B_SPLINE_CURVE_WITH_KNOTS('',3,(#25913,#25914,#25915,#25916,#25917,
#25918,#25919,#25920,#25921,#25922,#25923,#25924,#25925,#25926,#25927,#25928,
#25929,#25930,#25931,#25932,#25933,#25934),.UNSPECIFIED.,.F.,.F.,(4,3,3,
3,3,3,3,4),(-248.742942471708,-247.84081712438,-246.841458990814,-245.842100857247,
-244.842742723681,-243.843384590115,-242.844026456549,-242.459757164528),
 .UNSPECIFIED.);
#557=B_SPLINE_CURVE_WITH_KNOTS('',3,(#25935,#25936,#25937,#25938,#25939,
#25940,#25941,#25942,#25943,#25944,#25945,#25946,#25947,#25948,#25949,#25950,
#25951,#25952,#25953,#25954,#25955,#25956),.UNSPECIFIED.,.F.,.F.,(4,3,3,
3,3,3,3,4),(239.204102343378,239.845952055851,240.845310189417,241.844668322983,
242.84402645655,243.843384590116,244.842742723682,245.487287650558),
 .UNSPECIFIED.);
#558=B_SPLINE_CURVE_WITH_KNOTS('',3,(#25961,#25962,#25963,#25964,#25965,
#25966,#25967,#25968,#25969,#25970,#25971,#25972,#25973,#25974,#25975,#25976,
#25977,#25978,#25979,#25980,#25981,#25982,#25983,#25984,#25985),
 .UNSPECIFIED.,.F.,.F.,(4,3,3,3,3,3,3,3,4),(-255.026127778888,-254.836324059342,
-253.836965925776,-252.83760779221,-251.838249658644,-250.838891525078,
-249.839533391512,-248.840175257946,-248.742942471708),.UNSPECIFIED.);
#559=B_SPLINE_CURVE_WITH_KNOTS('',3,(#25986,#25987,#25988,#25989,#25990,
#25991,#25992,#25993,#25994,#25995,#25996,#25997,#25998,#25999,#26000,#26001,
#26002,#26003,#26004,#26005,#26006,#26007),.UNSPECIFIED.,.F.,.F.,(4,3,3,
3,3,3,3,4),(245.487287650558,245.842100857248,246.841458990814,247.84081712438,
248.840175257946,249.839533391512,250.838891525078,251.770472957738),
 .UNSPECIFIED.);
#560=B_SPLINE_CURVE_WITH_KNOTS('',3,(#26012,#26013,#26014,#26015,#26016,
#26017,#26018,#26019,#26020,#26021,#26022,#26023,#26024,#26025,#26026,#26027,
#26028,#26029,#26030,#26031,#26032,#26033),.UNSPECIFIED.,.F.,.F.,(4,3,3,
3,3,3,3,4),(-261.309313086067,-260.832472860738,-259.833114727172,-258.833756593606,
-257.83439846004,-256.835040326474,-255.835682192908,-255.026127778888),
 .UNSPECIFIED.);
#561=B_SPLINE_CURVE_WITH_KNOTS('',3,(#26034,#26035,#26036,#26037,#26038,
#26039,#26040,#26041,#26042,#26043,#26044,#26045,#26046,#26047,#26048,#26049,
#26050,#26051,#26052,#26053,#26054,#26055,#26056,#26057,#26058),
 .UNSPECIFIED.,.F.,.F.,(4,3,3,3,3,3,3,3,4),(251.770472957738,251.838249658644,
252.83760779221,253.836965925776,254.836324059342,255.835682192908,256.835040326474,
257.83439846004,258.053658264917),.UNSPECIFIED.);
#562=B_SPLINE_CURVE_WITH_KNOTS('',3,(#26063,#26064,#26065,#26066,#26067,
#26068,#26069,#26070,#26071,#26072,#26073,#26074,#26075,#26076,#26077,#26078,
#26079,#26080,#26081,#26082,#26083,#26084),.UNSPECIFIED.,.F.,.F.,(4,3,3,
3,3,3,3,4),(-267.592498393247,-266.828621662134,-265.829263528568,-264.829905395002,
-263.830547261436,-262.83118912787,-261.831830994304,-261.309313086067),
 .UNSPECIFIED.);
#563=B_SPLINE_CURVE_WITH_KNOTS('',3,(#26085,#26086,#26087,#26088,#26089,
#26090,#26091,#26092,#26093,#26094,#26095,#26096,#26097,#26098,#26099,#26100,
#26101,#26102,#26103,#26104,#26105,#26106),.UNSPECIFIED.,.F.,.F.,(4,3,3,
3,3,3,3,4),(258.053658264917,258.833756593606,259.833114727172,260.832472860738,
261.831830994304,262.83118912787,263.830547261436,264.336843572097),
 .UNSPECIFIED.);
#564=B_SPLINE_CURVE_WITH_KNOTS('',3,(#26111,#26112,#26113,#26114,#26115,
#26116,#26117,#26118,#26119,#26120,#26121,#26122,#26123,#26124,#26125,#26126,
#26127,#26128,#26129,#26130,#26131,#26132,#26133,#26134,#26135),
 .UNSPECIFIED.,.F.,.F.,(4,3,3,3,3,3,3,3,4),(-273.875683700426,-273.824128597097,
-272.824770463531,-271.825412329965,-270.826054196399,-269.826696062833,
-268.827337929266,-267.8279797957,-267.592498393247),.UNSPECIFIED.);
#565=B_SPLINE_CURVE_WITH_KNOTS('',3,(#26136,#26137,#26138,#26139,#26140,
#26141,#26142,#26143,#26144,#26145,#26146,#26147,#26148,#26149,#26150,#26151,
#26152,#26153,#26154,#26155,#26156,#26157),.UNSPECIFIED.,.F.,.F.,(4,3,3,
3,3,3,3,4),(264.336843572097,264.829905395003,265.829263528569,266.828621662135,
267.827979795701,268.827337929267,269.826696062833,270.620028879276),
 .UNSPECIFIED.);
#566=B_SPLINE_CURVE_WITH_KNOTS('',3,(#26162,#26163,#26164,#26165,#26166,
#26167,#26168,#26169,#26170,#26171,#26172,#26173,#26174,#26175,#26176,#26177,
#26178,#26179,#26180,#26181,#26182,#26183),.UNSPECIFIED.,.F.,.F.,(4,3,3,
3,3,3,3,4),(-280.158869007606,-279.820277398493,-278.820919264927,-277.821561131361,
-276.822202997795,-275.822844864229,-274.823486730663,-273.875683700426),
 .UNSPECIFIED.);
#567=B_SPLINE_CURVE_WITH_KNOTS('',3,(#26184,#26185,#26186,#26187,#26188,
#26189,#26190,#26191,#26192,#26193,#26194,#26195,#26196,#26197,#26198,#26199,
#26200,#26201,#26202,#26203,#26204,#26205,#26206,#26207,#26208),
 .UNSPECIFIED.,.F.,.F.,(4,3,3,3,3,3,3,3,4),(270.620028879276,270.826054196399,
271.825412329965,272.824770463531,273.824128597097,274.823486730663,275.822844864229,
276.822202997795,276.903214186456),.UNSPECIFIED.);
#568=B_SPLINE_CURVE_WITH_KNOTS('',3,(#26213,#26214,#26215,#26216,#26217,
#26218,#26219,#26220,#26221,#26222,#26223,#26224,#26225,#26226,#26227,#26228,
#26229,#26230,#26231,#26232,#26233,#26234),.UNSPECIFIED.,.F.,.F.,(4,3,3,
3,3,3,3,4),(-286.442054314785,-285.816426199889,-284.817068066323,-283.817709932757,
-282.818351799191,-281.818993665625,-280.819635532059,-280.158869007606),
 .UNSPECIFIED.);
#569=B_SPLINE_CURVE_WITH_KNOTS('',3,(#26235,#26236,#26237,#26238,#26239,
#26240,#26241,#26242,#26243,#26244,#26245,#26246,#26247,#26248,#26249,#26250,
#26251,#26252,#26253,#26254,#26255,#26256),.UNSPECIFIED.,.F.,.F.,(4,3,3,
3,3,3,3,4),(276.903214186456,277.821561131361,278.820919264927,279.820277398493,
280.819635532059,281.818993665625,282.818351799191,283.186399493635),
 .UNSPECIFIED.);
#570=B_SPLINE_CURVE_WITH_KNOTS('',3,(#26261,#26262,#26263,#26264,#26265,
#26266,#26267,#26268,#26269,#26270,#26271,#26272,#26273,#26274,#26275,#26276,
#26277,#26278,#26279,#26280,#26281,#26282),.UNSPECIFIED.,.F.,.F.,(4,3,3,
3,3,3,3,4),(-292.725239621965,-291.812575001286,-290.81321686772,-289.813858734153,
-288.814500600587,-287.815142467021,-286.815784333455,-286.442054314785),
 .UNSPECIFIED.);
#571=B_SPLINE_CURVE_WITH_KNOTS('',3,(#26283,#26284,#26285,#26286,#26287,
#26288,#26289,#26290,#26291,#26292,#26293,#26294,#26295,#26296,#26297,#26298,
#26299,#26300,#26301,#26302,#26303,#26304),.UNSPECIFIED.,.F.,.F.,(4,3,3,
3,3,3,3,4),(283.186399493635,283.817709932757,284.817068066323,285.81642619989,
286.815784333456,287.815142467022,288.814500600588,289.469584800815),
 .UNSPECIFIED.);
#572=B_SPLINE_CURVE_WITH_KNOTS('',3,(#26309,#26310,#26311,#26312,#26313,
#26314,#26315,#26316,#26317,#26318,#26319,#26320,#26321,#26322,#26323,#26324,
#26325,#26326,#26327,#26328,#26329,#26330,#26331,#26332,#26333),
 .UNSPECIFIED.,.F.,.F.,(4,3,3,3,3,3,3,3,4),(-299.008424929145,-298.808081936248,
-297.808723802682,-296.809365669116,-295.81000753555,-294.810649401984,
-293.811291268418,-292.811933134852,-292.725239621965),.UNSPECIFIED.);
#573=B_SPLINE_CURVE_WITH_KNOTS('',3,(#26334,#26335,#26336,#26337,#26338,
#26339,#26340,#26341,#26342,#26343,#26344,#26345,#26346,#26347,#26348,#26349,
#26350,#26351,#26352,#26353,#26354,#26355),.UNSPECIFIED.,.F.,.F.,(4,3,3,
3,3,3,3,4),(289.469584800815,289.813858734154,290.81321686772,291.812575001286,
292.811933134852,293.811291268418,294.810649401984,295.752770107995),
 .UNSPECIFIED.);
#574=B_SPLINE_CURVE_WITH_KNOTS('',3,(#26360,#26361,#26362,#26363,#26364,
#26365,#26366,#26367,#26368,#26369,#26370,#26371,#26372,#26373,#26374,#26375,
#26376,#26377,#26378,#26379,#26380,#26381),.UNSPECIFIED.,.F.,.F.,(4,3,3,
3,3,3,3,4),(-305.291610236324,-304.804230737644,-303.804872604078,-302.805514470512,
-301.806156336946,-300.80679820338,-299.807440069814,-299.008424929145),
 .UNSPECIFIED.);
#575=B_SPLINE_CURVE_WITH_KNOTS('',3,(#26382,#26383,#26384,#26385,#26386,
#26387,#26388,#26389,#26390,#26391,#26392,#26393,#26394,#26395,#26396,#26397,
#26398,#26399,#26400,#26401,#26402,#26403,#26404,#26405,#26406),
 .UNSPECIFIED.,.F.,.F.,(4,3,3,3,3,3,3,3,4),(295.752770107995,295.81000753555,
296.809365669116,297.808723802682,298.808081936248,299.807440069814,300.80679820338,
301.806156336946,302.035955415174),.UNSPECIFIED.);
#576=B_SPLINE_CURVE_WITH_KNOTS('',3,(#26411,#26412,#26413,#26414,#26415,
#26416,#26417,#26418,#26419,#26420,#26421,#26422,#26423,#26424,#26425,#26426,
#26427,#26428,#26429,#26430,#26431,#26432),.UNSPECIFIED.,.F.,.F.,(4,3,3,
3,3,3,3,4),(-311.574795543504,-310.80037953904,-309.801021405475,-308.801663271908,
-307.802305138342,-306.802947004776,-305.80358887121,-305.291610236324),
 .UNSPECIFIED.);
#577=B_SPLINE_CURVE_WITH_KNOTS('',3,(#26433,#26434,#26435,#26436,#26437,
#26438,#26439,#26440,#26441,#26442,#26443,#26444,#26445,#26446,#26447,#26448,
#26449,#26450,#26451,#26452,#26453,#26454),.UNSPECIFIED.,.F.,.F.,(4,3,3,
3,3,3,3,4),(302.035955415174,302.805514470512,303.804872604078,304.804230737644,
305.80358887121,306.802947004777,307.802305138343,308.319140722354),
 .UNSPECIFIED.);
#578=B_SPLINE_CURVE_WITH_KNOTS('',3,(#26459,#26460,#26461,#26462,#26463,
#26464,#26465,#26466,#26467,#26468,#26469,#26470,#26471,#26472,#26473,#26474,
#26475,#26476,#26477,#26478,#26479,#26480,#26481,#26482,#26483),
 .UNSPECIFIED.,.F.,.F.,(4,3,3,3,3,3,3,3,4),(-317.857980850683,-317.795886474003,
-316.796528340437,-315.797170206871,-314.797812073305,-313.798453939739,
-312.799095806173,-311.799737672607,-311.574795543504),.UNSPECIFIED.);
#579=B_SPLINE_CURVE_WITH_KNOTS('',3,(#26484,#26485,#26486,#26487,#26488,
#26489,#26490,#26491,#26492,#26493,#26494,#26495,#26496,#26497,#26498,#26499,
#26500,#26501,#26502,#26503,#26504,#26505),.UNSPECIFIED.,.F.,.F.,(4,3,3,
3,3,3,3,4),(308.319140722354,308.801663271909,309.801021405475,310.800379539041,
311.799737672607,312.799095806173,313.798453939739,314.602326029533),
 .UNSPECIFIED.);
#580=B_SPLINE_CURVE_WITH_KNOTS('',3,(#26510,#26511,#26512,#26513,#26514,
#26515,#26516,#26517,#26518,#26519,#26520,#26521,#26522,#26523,#26524,#26525,
#26526,#26527,#26528,#26529,#26530,#26531),.UNSPECIFIED.,.F.,.F.,(4,3,3,
3,3,3,3,4),(-324.141166157863,-323.792035275399,-322.792677141833,-321.793319008267,
-320.793960874701,-319.794602741135,-318.795244607569,-317.857980850683),
 .UNSPECIFIED.);
#581=B_SPLINE_CURVE_WITH_KNOTS('',3,(#26532,#26533,#26534,#26535,#26536,
#26537,#26538,#26539,#26540,#26541,#26542,#26543,#26544,#26545,#26546,#26547,
#26548,#26549,#26550,#26551,#26552,#26553,#26554,#26555,#26556),
 .UNSPECIFIED.,.F.,.F.,(4,3,3,3,3,3,3,3,4),(314.602326029533,314.797812073305,
315.797170206871,316.796528340437,317.795886474003,318.795244607569,319.794602741135,
320.793960874701,320.885511336713),.UNSPECIFIED.);
#582=B_SPLINE_CURVE_WITH_KNOTS('',3,(#26561,#26562,#26563,#26564,#26565,
#26566,#26567,#26568,#26569,#26570,#26571,#26572,#26573,#26574,#26575,#26576,
#26577,#26578,#26579,#26580,#26581,#26582),.UNSPECIFIED.,.F.,.F.,(4,3,3,
3,3,3,3,4),(-330.424351465042,-329.788184076795,-328.788825943229,-327.789467809663,
-326.790109676097,-325.790751542531,-324.791393408965,-324.141166157863),
 .UNSPECIFIED.);
#583=B_SPLINE_CURVE_WITH_KNOTS('',3,(#26583,#26584,#26585,#26586,#26587,
#26588,#26589,#26590,#26591,#26592,#26593,#26594,#26595,#26596,#26597,#26598,
#26599,#26600,#26601,#26602,#26603,#26604),.UNSPECIFIED.,.F.,.F.,(4,3,3,
3,3,3,3,4),(320.885511336713,321.793319008267,322.792677141833,323.792035275399,
324.791393408965,325.790751542531,326.790109676097,327.168696643892),
 .UNSPECIFIED.);
#584=B_SPLINE_CURVE_WITH_KNOTS('',3,(#26609,#26610,#26611,#26612,#26613,
#26614,#26615,#26616,#26617,#26618,#26619,#26620,#26621,#26622,#26623,#26624,
#26625,#26626,#26627,#26628,#26629,#26630),.UNSPECIFIED.,.F.,.F.,(4,3,3,
3,3,3,3,4),(-336.707536772222,-335.784332878192,-334.784974744626,-333.78561661106,
-332.786258477494,-331.786900343927,-330.787542210361,-330.424351465042),
 .UNSPECIFIED.);
#585=B_SPLINE_CURVE_WITH_KNOTS('',3,(#26631,#26632,#26633,#26634,#26635,
#26636,#26637,#26638,#26639,#26640,#26641,#26642,#26643,#26644,#26645,#26646,
#26647,#26648,#26649,#26650,#26651,#26652),.UNSPECIFIED.,.F.,.F.,(4,3,3,
3,3,3,3,4),(327.168696643892,327.789467809663,328.78882594323,329.788184076796,
330.787542210362,331.786900343928,332.786258477494,333.451881951072),
 .UNSPECIFIED.);
#586=B_SPLINE_CURVE_WITH_KNOTS('',3,(#26657,#26658,#26659,#26660,#26661,
#26662,#26663,#26664,#26665,#26666,#26667,#26668,#26669,#26670,#26671,#26672,
#26673,#26674,#26675,#26676,#26677,#26678,#26679,#26680,#26681),
 .UNSPECIFIED.,.F.,.F.,(4,3,3,3,3,3,3,3,4),(-342.990722079402,-342.779839813154,
-341.780481679588,-340.781123546022,-339.781765412456,-338.78240727889,
-337.783049145324,-336.783691011758,-336.707536772222),.UNSPECIFIED.);
#587=B_SPLINE_CURVE_WITH_KNOTS('',3,(#26682,#26683,#26684,#26685,#26686,
#26687,#26688,#26689,#26690,#26691,#26692,#26693,#26694,#26695,#26696,#26697,
#26698,#26699,#26700,#26701,#26702,#26703),.UNSPECIFIED.,.F.,.F.,(4,3,3,
3,3,3,3,4),(333.451881951072,333.78561661106,334.784974744626,335.784332878192,
336.783691011758,337.783049145324,338.78240727889,339.735067258252),
 .UNSPECIFIED.);
#588=B_SPLINE_CURVE_WITH_KNOTS('',3,(#26708,#26709,#26710,#26711,#26712,
#26713,#26714,#26715,#26716,#26717,#26718,#26719,#26720,#26721,#26722,#26723,
#26724,#26725,#26726,#26727,#26728,#26729,#26730,#26731,#26732,#26733,#26734,
#26735,#26736,#26737,#26738,#26739,#26740,#26741),.UNSPECIFIED.,.F.,.F.,
(4,3,3,3,3,3,3,3,3,3,3,4),(-349.273907386581,-348.77598861455,-348.276309547767,
-347.776630480984,-347.276951414201,-346.777272347418,-346.277593280635,
-345.777914213852,-345.278235147069,-344.778556080286,-343.77919794672,
-342.990722079402),.UNSPECIFIED.);
#589=B_SPLINE_CURVE_WITH_KNOTS('',3,(#26742,#26743,#26744,#26745,#26746,
#26747,#26748,#26749,#26750,#26751,#26752,#26753,#26754,#26755,#26756,#26757,
#26758,#26759,#26760,#26761,#26762,#26763,#26764,#26765,#26766,#26767,#26768,
#26769),.UNSPECIFIED.,.F.,.F.,(4,3,3,3,3,3,3,3,3,4),(339.735067258252,339.781765412456,
340.781123546022,341.780481679588,342.779839813154,343.77919794672,344.778556080286,
345.278235147069,345.777914213852,346.018252565431),.UNSPECIFIED.);
#590=B_SPLINE_CURVE_WITH_KNOTS('',3,(#26774,#26775,#26776,#26777,#26778,
#26779,#26780,#26781,#26782,#26783,#26784,#26785,#26786,#26787,#26788,#26789,
#26790,#26791,#26792,#26793,#26794,#26795,#26796,#26797,#26798,#26799,#26800,
#26801,#26802,#26803,#26804,#26805,#26806,#26807,#26808,#26809,#26810,#26811,
#26812,#26813,#26814,#26815,#26816),.UNSPECIFIED.,.F.,.F.,(4,3,3,3,3,3,
3,3,3,3,3,3,3,3,4),(-355.557092693761,-355.27181648273,-354.772137415947,
-354.272458349164,-353.77277928238,-353.273100215597,-352.773421148814,
-352.273742082031,-351.774063015248,-351.274383948465,-350.774704881682,
-350.275025814899,-349.775346748116,-349.275667681333,-349.273907386581),
 .UNSPECIFIED.);
#591=B_SPLINE_CURVE_WITH_KNOTS('',3,(#26817,#26818,#26819,#26820,#26821,
#26822,#26823,#26824,#26825,#26826,#26827,#26828,#26829,#26830,#26831,#26832,
#26833,#26834,#26835,#26836,#26837,#26838,#26839,#26840,#26841,#26842,#26843,
#26844,#26845,#26846,#26847,#26848,#26849,#26850,#26851,#26852,#26853,#26854,
#26855,#26856,#26857,#26858,#26859),.UNSPECIFIED.,.F.,.F.,(4,3,3,3,3,3,
3,3,3,3,3,3,3,3,4),(346.018252565431,346.277593280635,346.777272347418,
347.276951414201,347.776630480984,348.276309547767,348.77598861455,349.275667681334,
349.775346748116,350.2750258149,350.774704881683,351.274383948466,351.774063015249,
352.273742082032,352.301437872611),.UNSPECIFIED.);
#592=B_SPLINE_CURVE_WITH_KNOTS('',3,(#26864,#26865,#26866,#26867,#26868,
#26869,#26870,#26871,#26872,#26873,#26874,#26875,#26876,#26877,#26878,#26879,
#26880,#26881,#26882,#26883,#26884,#26885,#26886,#26887,#26888,#26889,#26890,
#26891,#26892,#26893,#26894,#26895,#26896,#26897,#26898,#26899,#26900,#26901,
#26902,#26903,#26904,#26905,#26906),.UNSPECIFIED.,.F.,.F.,(4,3,3,3,3,3,
3,3,3,3,3,3,3,3,4),(-361.84027800094,-361.767644350909,-361.267965284126,
-360.768286217343,-360.26860715056,-359.768928083777,-359.269249016994,
-358.769569950211,-358.269890883428,-357.770211816645,-357.270532749862,
-356.770853683079,-356.271174616296,-355.771495549513,-355.557092693761),
 .UNSPECIFIED.);
#593=B_SPLINE_CURVE_WITH_KNOTS('',3,(#26907,#26908,#26909,#26910,#26911,
#26912,#26913,#26914,#26915,#26916,#26917,#26918,#26919,#26920,#26921,#26922,
#26923,#26924,#26925,#26926,#26927,#26928,#26929,#26930,#26931,#26932,#26933,
#26934,#26935,#26936,#26937,#26938,#26939,#26940,#26941,#26942,#26943,#26944,
#26945,#26946),.UNSPECIFIED.,.F.,.F.,(4,3,3,3,3,3,3,3,3,3,3,3,3,4),(352.301437872611,
352.773421148815,353.273100215598,353.772779282381,354.272458349164,354.772137415947,
355.27181648273,355.771495549513,356.271174616296,356.770853683079,357.270532749862,
357.770211816645,358.269890883428,358.58462317979),.UNSPECIFIED.);
#594=B_SPLINE_CURVE_WITH_KNOTS('',3,(#26951,#26952,#26953,#26954,#26955,
#26956,#26957,#26958,#26959,#26960,#26961,#26962,#26963,#26964,#26965,#26966,
#26967,#26968,#26969,#26970,#26971,#26972,#26973,#26974,#26975,#26976,#26977,
#26978,#26979,#26980,#26981,#26982,#26983,#26984,#26985,#26986,#26987,#26988,
#26989,#26990),.UNSPECIFIED.,.F.,.F.,(4,3,3,3,3,3,3,3,3,3,3,3,3,4),(-368.12346330812,
-367.763793152305,-367.264114085522,-366.764435018739,-366.264755951956,
-365.765076885173,-365.26539781839,-364.765718751607,-364.266039684824,
-363.766360618041,-363.266681551258,-362.767002484475,-362.267323417692,
-361.84027800094),.UNSPECIFIED.);
#595=B_SPLINE_CURVE_WITH_KNOTS('',3,(#26991,#26992,#26993,#26994,#26995,
#26996,#26997,#26998,#26999,#27000,#27001,#27002,#27003,#27004,#27005,#27006,
#27007,#27008,#27009,#27010,#27011,#27012,#27013,#27014,#27015,#27016,#27017,
#27018,#27019,#27020,#27021,#27022,#27023,#27024,#27025,#27026,#27027,#27028,
#27029,#27030,#27031,#27032,#27033),.UNSPECIFIED.,.F.,.F.,(4,3,3,3,3,3,
3,3,3,3,3,3,3,3,4),(358.58462317979,358.769569950211,359.269249016994,359.768928083777,
360.26860715056,360.768286217343,361.267965284126,361.767644350909,362.267323417692,
362.767002484475,363.266681551258,363.766360618041,364.266039684824,364.765718751607,
364.86780848697),.UNSPECIFIED.);
#596=B_SPLINE_CURVE_WITH_KNOTS('',3,(#27038,#27039,#27040,#27041,#27042,
#27043,#27044,#27045,#27046,#27047,#27048,#27049,#27050,#27051,#27052,#27053,
#27054,#27055,#27056,#27057,#27058,#27059,#27060,#27061,#27062,#27063,#27064,
#27065,#27066,#27067,#27068,#27069,#27070,#27071,#27072,#27073,#27074,#27075,
#27076,#27077,#27078,#27079,#27080),.UNSPECIFIED.,.F.,.F.,(4,3,3,3,3,3,
3,3,3,3,3,3,3,3,4),(-374.406648615299,-374.259621020484,-373.759941953701,
-373.260262886918,-372.760583820135,-372.260904753352,-371.761225686569,
-371.261546619786,-370.761867553003,-370.26218848622,-369.762509419437,
-369.262830352654,-368.763151285871,-368.263472219088,-368.12346330812),
 .UNSPECIFIED.);
#597=B_SPLINE_CURVE_WITH_KNOTS('',3,(#27081,#27082,#27083,#27084,#27085,
#27086,#27087,#27088,#27089,#27090,#27091,#27092,#27093,#27094,#27095,#27096,
#27097,#27098,#27099,#27100,#27101,#27102,#27103,#27104,#27105,#27106,#27107,
#27108,#27109,#27110,#27111,#27112,#27113,#27114,#27115,#27116,#27117,#27118,
#27119,#27120),.UNSPECIFIED.,.F.,.F.,(4,3,3,3,3,3,3,3,3,3,3,3,3,4),(364.86780848697,
365.26539781839,365.765076885173,366.264755951956,366.764435018739,367.264114085522,
367.763793152305,368.263472219088,368.763151285871,369.262830352654,369.762509419437,
370.26218848622,370.761867553004,371.150993794149),.UNSPECIFIED.);
#598=B_SPLINE_CURVE_WITH_KNOTS('',3,(#27125,#27126,#27127,#27128,#27129,
#27130,#27131,#27132,#27133,#27134,#27135,#27136,#27137,#27138,#27139,#27140,
#27141,#27142,#27143,#27144,#27145,#27146,#27147,#27148,#27149,#27150,#27151,
#27152,#27153,#27154,#27155,#27156,#27157,#27158,#27159,#27160,#27161,#27162,
#27163,#27164),.UNSPECIFIED.,.F.,.F.,(4,3,3,3,3,3,3,3,3,3,3,3,3,4),(-380.689833922479,
-380.255769821881,-379.756090755098,-379.256411688315,-378.756732621532,
-378.257053554749,-377.757374487966,-377.257695421183,-376.7580163544,-376.258337287616,
-375.758658220834,-375.25897915405,-374.759300087267,-374.406648615299),
 .UNSPECIFIED.);
#599=B_SPLINE_CURVE_WITH_KNOTS('',3,(#27165,#27166,#27167,#27168,#27169,
#27170,#27171,#27172,#27173,#27174,#27175,#27176,#27177,#27178,#27179,#27180,
#27181,#27182,#27183,#27184,#27185,#27186,#27187,#27188,#27189,#27190,#27191,
#27192,#27193,#27194,#27195,#27196,#27197,#27198,#27199,#27200,#27201,#27202,
#27203,#27204,#27205,#27206,#27207),.UNSPECIFIED.,.F.,.F.,(4,3,3,3,3,3,
3,3,3,3,3,3,3,3,4),(371.150993794149,371.261546619787,371.76122568657,372.260904753353,
372.760583820136,373.260262886919,373.759941953702,374.259621020485,374.759300087268,
375.258979154051,375.758658220834,376.258337287617,376.7580163544,377.257695421183,
377.434179101329),.UNSPECIFIED.);
#600=B_SPLINE_CURVE_WITH_KNOTS('',3,(#27212,#27213,#27214,#27215,#27216,
#27217,#27218,#27219,#27220,#27221,#27222,#27223,#27224,#27225,#27226,#27227,
#27228,#27229,#27230,#27231,#27232,#27233,#27234,#27235,#27236,#27237,#27238,
#27239,#27240,#27241,#27242,#27243,#27244,#27245,#27246,#27247,#27248,#27249,
#27250,#27251,#27252,#27253,#27254),.UNSPECIFIED.,.F.,.F.,(4,3,3,3,3,3,
3,3,3,3,3,3,3,3,4),(-386.973019229658,-386.75159769006,-386.251918623277,
-385.752239556494,-385.252560489711,-384.752881422928,-384.253202356145,
-383.753523289362,-383.253844222579,-382.754165155796,-382.254486089013,
-381.75480702223,-381.255127955447,-380.755448888664,-380.689833922479),
 .UNSPECIFIED.);
#601=B_SPLINE_CURVE_WITH_KNOTS('',3,(#27255,#27256,#27257,#27258,#27259,
#27260,#27261,#27262,#27263,#27264,#27265,#27266,#27267,#27268,#27269,#27270,
#27271,#27272,#27273,#27274,#27275,#27276,#27277,#27278,#27279,#27280,#27281,
#27282,#27283,#27284,#27285,#27286,#27287,#27288,#27289,#27290,#27291,#27292,
#27293,#27294),.UNSPECIFIED.,.F.,.F.,(4,3,3,3,3,3,3,3,3,3,3,3,3,4),(377.434179101329,
377.757374487966,378.257053554749,378.756732621532,379.256411688315,379.756090755098,
380.255769821881,380.755448888664,381.255127955447,381.75480702223,382.254486089013,
382.754165155796,383.253844222579,383.717364408508),.UNSPECIFIED.);
#602=B_SPLINE_CURVE_WITH_KNOTS('',3,(#27299,#27300,#27301,#27302,#27303,
#27304,#27305,#27306,#27307,#27308,#27309,#27310,#27311,#27312,#27313,#27314,
#27315,#27316,#27317,#27318,#27319,#27320,#27321,#27322,#27323,#27324,#27325,
#27326,#27327,#27328,#27329,#27330,#27331,#27332,#27333,#27334,#27335,#27336,
#27337,#27338,#27339,#27340,#27341),.UNSPECIFIED.,.F.,.F.,(4,3,3,3,3,3,
3,3,3,3,3,3,3,3,4),(-393.256204536838,-393.247425558239,-392.747746491456,
-392.248067424673,-391.74838835789,-391.248709291107,-390.749030224324,
-390.249351157541,-389.749672090758,-389.249993023975,-388.750313957192,
-388.250634890409,-387.750955823626,-387.251276756843,-386.973019229658),
 .UNSPECIFIED.);
#603=B_SPLINE_CURVE_WITH_KNOTS('',3,(#27342,#27343,#27344,#27345,#27346,
#27347,#27348,#27349,#27350,#27351,#27352,#27353,#27354,#27355,#27356,#27357,
#27358,#27359,#27360,#27361,#27362,#27363,#27364,#27365,#27366,#27367,#27368,
#27369,#27370,#27371,#27372,#27373,#27374,#27375,#27376,#27377,#27378,#27379,
#27380,#27381,#27382,#27383,#27384),.UNSPECIFIED.,.F.,.F.,(4,3,3,3,3,3,
3,3,3,3,3,3,3,3,4),(383.717364408508,383.753523289362,384.253202356145,
384.752881422928,385.252560489711,385.752239556494,386.251918623277,386.75159769006,
387.251276756843,387.750955823626,388.250634890409,388.750313957192,389.249993023975,
389.749672090758,390.000549715688),.UNSPECIFIED.);
#604=B_SPLINE_CURVE_WITH_KNOTS('',3,(#27390,#27391,#27392,#27393),
 .UNSPECIFIED.,.F.,.F.,(4,4),(405.265452313083,405.755527026166),
 .UNSPECIFIED.);
#605=B_SPLINE_CURVE_WITH_KNOTS('',3,(#27399,#27400,#27401,#27402,#27403,
#27404,#27405,#27406,#27407,#27408,#27409,#27410,#27411,#27412,#27413,#27414,
#27415),.UNSPECIFIED.,.F.,.F.,(4,1,1,1,1,1,1,1,1,1,1,1,1,1,4),(398.982267005903,
399.260524533088,399.760203599871,400.259882666654,400.759561733437,401.25924080022,
401.758919867003,402.258598933787,402.75827800057,403.257957067353,403.757636134136,
404.257315200919,404.756994267702,405.256673334485,405.265452313083),
 .UNSPECIFIED.);
#606=B_SPLINE_CURVE_WITH_KNOTS('',3,(#27418,#27419,#27420,#27421,#27422,
#27423,#27424,#27425,#27426,#27427,#27428,#27429,#27430),.UNSPECIFIED.,
 .F.,.F.,(4,1,1,1,1,1,1,1,1,1,4),(398.982267005904,399.231068447758,399.730747514541,
400.230426581324,400.730105648107,401.22978471489,401.729463781673,402.229142848456,
402.728821915239,403.228500982022,403.728180048805),.UNSPECIFIED.);
#607=B_SPLINE_CURVE_WITH_KNOTS('',3,(#27435,#27436,#27437,#27438,#27439,
#27440,#27441,#27442,#27443,#27444,#27445,#27446,#27447,#27448,#27449,#27450,
#27451),.UNSPECIFIED.,.F.,.F.,(4,1,1,1,1,1,1,1,1,1,1,1,1,1,4),(392.699081698724,
392.764696664909,393.264375731692,393.764054798475,394.263733865258,394.763412932041,
395.263091998824,395.762771065607,396.26245013239,396.762129199173,397.261808265956,
397.761487332739,398.261166399522,398.760845466305,398.982267005903),
 .UNSPECIFIED.);
#608=B_SPLINE_CURVE_WITH_KNOTS('',3,(#27452,#27453,#27454,#27455,#27456,
#27457,#27458,#27459,#27460,#27461,#27462,#27463,#27464,#27465,#27466,#27467,
#27468),.UNSPECIFIED.,.F.,.F.,(4,1,1,1,1,1,1,1,1,1,1,1,1,1,4),(392.699081698724,
392.735240579579,393.234919646362,393.734598713145,394.234277779928,394.733956846711,
395.233635913494,395.733314980277,396.23299404706,396.732673113843,397.232352180626,
397.732031247409,398.231710314192,398.731389380975,398.982267005904),
 .UNSPECIFIED.);
#609=B_SPLINE_CURVE_WITH_KNOTS('',3,(#27473,#27474,#27475,#27476,#27477,
#27478,#27479,#27480,#27481,#27482,#27483,#27484,#27485,#27486,#27487,#27488),
 .UNSPECIFIED.,.F.,.F.,(4,1,1,1,1,1,1,1,1,1,1,1,1,4),(386.415896391544,
386.768547863513,387.268226930296,387.767905997079,388.267585063862,388.767264130645,
389.266943197428,389.766622264211,390.266301330994,390.765980397777,391.26565946456,
391.765338531343,392.265017598126,392.699081698724),.UNSPECIFIED.);
#610=B_SPLINE_CURVE_WITH_KNOTS('',3,(#27489,#27490,#27491,#27492,#27493,
#27494,#27495,#27496,#27497,#27498,#27499,#27500,#27501,#27502,#27503,#27504),
 .UNSPECIFIED.,.F.,.F.,(4,1,1,1,1,1,1,1,1,1,1,1,1,4),(386.415896391545,
386.739091778183,387.238770844966,387.738449911749,388.238128978532,388.737808045315,
389.237487112098,389.737166178881,390.236845245664,390.736524312447,391.23620337923,
391.735882446013,392.235561512796,392.699081698724),.UNSPECIFIED.);
#611=B_SPLINE_CURVE_WITH_KNOTS('',3,(#27509,#27510,#27511,#27512,#27513,
#27514,#27515,#27516,#27517,#27518,#27519,#27520,#27521,#27522,#27523,#27524,
#27525),.UNSPECIFIED.,.F.,.F.,(4,1,1,1,1,1,1,1,1,1,1,1,1,1,4),(380.132711084365,
380.272719995333,380.772399062117,381.2720781289,381.771757195683,382.271436262466,
382.771115329249,383.270794396032,383.770473462815,384.270152529598,384.769831596381,
385.269510663164,385.769189729947,386.26886879673,386.415896391544),
 .UNSPECIFIED.);
#612=B_SPLINE_CURVE_WITH_KNOTS('',3,(#27526,#27527,#27528,#27529,#27530,
#27531,#27532,#27533,#27534,#27535,#27536,#27537,#27538,#27539,#27540,#27541,
#27542),.UNSPECIFIED.,.F.,.F.,(4,1,1,1,1,1,1,1,1,1,1,1,1,1,4),(380.132711084365,
380.243263910003,380.742942976786,381.242622043569,381.742301110352,382.241980177135,
382.741659243918,383.241338310702,383.741017377485,384.240696444268,384.740375511051,
385.240054577834,385.739733644617,386.2394127114,386.415896391545),
 .UNSPECIFIED.);
#613=B_SPLINE_CURVE_WITH_KNOTS('',3,(#27547,#27548,#27549,#27550,#27551,
#27552,#27553,#27554,#27555,#27556,#27557,#27558,#27559,#27560,#27561,#27562),
 .UNSPECIFIED.,.F.,.F.,(4,1,1,1,1,1,1,1,1,1,1,1,1,4),(373.849525777185,
374.276571193937,374.77625026072,375.275929327503,375.775608394286,376.275287461069,
376.774966527852,377.274645594635,377.774324661418,378.274003728201,378.773682794984,
379.273361861767,379.77304092855,380.132711084365),.UNSPECIFIED.);
#614=B_SPLINE_CURVE_WITH_KNOTS('',3,(#27563,#27564,#27565,#27566,#27567,
#27568,#27569,#27570,#27571,#27572,#27573,#27574,#27575,#27576,#27577,#27578),
 .UNSPECIFIED.,.F.,.F.,(4,1,1,1,1,1,1,1,1,1,1,1,1,4),(373.849525777185,
374.247115108607,374.74679417539,375.246473242173,375.746152308956,376.245831375739,
376.745510442522,377.245189509305,377.744868576088,378.244547642871,378.744226709654,
379.243905776437,379.74358484322,380.132711084365),.UNSPECIFIED.);
#615=B_SPLINE_CURVE_WITH_KNOTS('',3,(#27583,#27584,#27585,#27586,#27587,
#27588,#27589,#27590,#27591,#27592,#27593,#27594,#27595,#27596,#27597,#27598,
#27599),.UNSPECIFIED.,.F.,.F.,(4,1,1,1,1,1,1,1,1,1,1,1,1,1,4),(367.566340470006,
367.780743325758,368.280422392541,368.780101459324,369.279780526107,369.77945959289,
370.279138659673,370.778817726456,371.278496793239,371.778175860022,372.277854926805,
372.777533993588,373.277213060371,373.776892127154,373.849525777185),
 .UNSPECIFIED.);
#616=B_SPLINE_CURVE_WITH_KNOTS('',3,(#27600,#27601,#27602,#27603,#27604,
#27605,#27606,#27607,#27608,#27609,#27610,#27611,#27612,#27613,#27614,#27615,
#27616),.UNSPECIFIED.,.F.,.F.,(4,1,1,1,1,1,1,1,1,1,1,1,1,1,4),(367.566340470006,
367.751287240428,368.250966307211,368.750645373994,369.250324440777,369.75000350756,
370.249682574343,370.749361641126,371.249040707909,371.748719774692,372.248398841475,
372.748077908258,373.247756975041,373.747436041824,373.849525777185),
 .UNSPECIFIED.);
#617=B_SPLINE_CURVE_WITH_KNOTS('',3,(#27621,#27622,#27623,#27624,#27625,
#27626,#27627,#27628,#27629,#27630,#27631,#27632,#27633,#27634,#27635,#27636,
#27637),.UNSPECIFIED.,.F.,.F.,(4,1,1,1,1,1,1,1,1,1,1,1,1,1,4),(361.283155162826,
361.284915457579,361.784594524362,362.284273591145,362.783952657928,363.283631724711,
363.783310791494,364.282989858277,364.78266892506,365.282347991843,365.782027058626,
366.281706125409,366.781385192192,367.281064258975,367.566340470006),
 .UNSPECIFIED.);
#618=B_SPLINE_CURVE_WITH_KNOTS('',3,(#27638,#27639,#27640,#27641,#27642,
#27643,#27644,#27645,#27646,#27647,#27648,#27649,#27650,#27651,#27652,#27653),
 .UNSPECIFIED.,.F.,.F.,(4,1,1,1,1,1,1,1,1,1,1,1,1,4),(361.283155162826,
361.755138439031,362.254817505815,362.754496572598,363.254175639381,363.753854706164,
364.253533772947,364.75321283973,365.252891906513,365.752570973296,366.252250040079,
366.751929106862,367.251608173645,367.566340470006),.UNSPECIFIED.);
#619=B_SPLINE_CURVE_WITH_KNOTS('',3,(#27658,#27659,#27660,#27661,#27662,
#27663,#27664,#27665,#27666,#27667,#27668,#27669,#27670,#27671),
 .UNSPECIFIED.,.F.,.F.,(4,1,1,1,1,1,1,1,1,1,1,4),(354.999969855646,355.788445722965,
356.787803856531,357.287482923314,357.787161990097,358.28684105688,358.786520123663,
359.286199190446,359.78587825723,360.285557324013,360.785236390796,361.283155162826),
 .UNSPECIFIED.);
#620=B_SPLINE_CURVE_WITH_KNOTS('',3,(#27672,#27673,#27674,#27675,#27676,
#27677,#27678,#27679,#27680,#27681,#27682,#27683,#27684,#27685,#27686,#27687,
#27688),.UNSPECIFIED.,.F.,.F.,(4,1,1,1,1,1,1,1,1,1,1,1,1,1,4),(354.999969855647,
355.259310570852,355.758989637635,356.258668704418,356.758347771201,357.258026837984,
357.757705904767,358.25738497155,358.757064038333,359.256743105116,359.756422171899,
360.256101238682,360.755780305465,361.255459372248,361.283155162826),
 .UNSPECIFIED.);
#621=B_SPLINE_CURVE_WITH_KNOTS('',3,(#27693,#27694,#27695,#27696,#27697,
#27698,#27699,#27700,#27701,#27702,#27703),.UNSPECIFIED.,.F.,.F.,(4,1,1,
1,1,1,1,1,4),(348.716784548467,348.792938788003,349.792296921569,350.791655055135,
351.791013188701,352.790371322267,353.789729455833,354.789087589399,354.999969855646),
 .UNSPECIFIED.);
#622=B_SPLINE_CURVE_WITH_KNOTS('',3,(#27704,#27705,#27706,#27707,#27708,
#27709,#27710,#27711,#27712,#27713,#27714,#27715),.UNSPECIFIED.,.F.,.F.,
(4,1,1,1,1,1,1,1,1,4),(348.716784548467,348.763482702673,349.762840836239,
350.762198969805,351.761557103371,352.760915236937,353.760273370503,354.259952437286,
354.759631504069,354.999969855647),.UNSPECIFIED.);
#623=B_SPLINE_CURVE_WITH_KNOTS('',3,(#27720,#27721,#27722,#27723,#27724,
#27725,#27726,#27727,#27728,#27729),.UNSPECIFIED.,.F.,.F.,(4,1,1,1,1,1,
1,4),(342.433599241287,342.796789986607,343.796148120173,344.795506253739,
345.794864387305,346.794222520871,347.793580654437,348.716784548467),
 .UNSPECIFIED.);
#624=B_SPLINE_CURVE_WITH_KNOTS('',3,(#27730,#27731,#27732,#27733,#27734,
#27735,#27736,#27737,#27738,#27739),.UNSPECIFIED.,.F.,.F.,(4,1,1,1,1,1,
1,4),(342.433599241288,342.767333901277,343.766692034843,344.766050168409,
345.765408301975,346.764766435541,347.764124569107,348.716784548467),
 .UNSPECIFIED.);
#625=B_SPLINE_CURVE_WITH_KNOTS('',3,(#27744,#27745,#27746,#27747,#27748,
#27749,#27750,#27751,#27752,#27753),.UNSPECIFIED.,.F.,.F.,(4,1,1,1,1,1,
1,4),(336.150413934108,336.80064118521,337.799999318776,338.799357452343,
339.798715585909,340.798073719475,341.797431853041,342.433599241287),
 .UNSPECIFIED.);
#626=B_SPLINE_CURVE_WITH_KNOTS('',3,(#27754,#27755,#27756,#27757,#27758,
#27759,#27760,#27761,#27762,#27763),.UNSPECIFIED.,.F.,.F.,(4,1,1,1,1,1,
1,4),(336.150413934108,336.77118509988,337.770543233446,338.769901367012,
339.769259500578,340.768617634145,341.767975767711,342.433599241288),
 .UNSPECIFIED.);
#627=B_SPLINE_CURVE_WITH_KNOTS('',3,(#27768,#27769,#27770,#27771,#27772,
#27773,#27774,#27775,#27776,#27777),.UNSPECIFIED.,.F.,.F.,(4,1,1,1,1,1,
1,4),(329.867228626928,330.804492383814,331.80385051738,332.803208650946,
333.802566784512,334.801924918078,335.801283051644,336.150413934108),
 .UNSPECIFIED.);
#628=B_SPLINE_CURVE_WITH_KNOTS('',3,(#27778,#27779,#27780,#27781,#27782,
#27783,#27784,#27785,#27786,#27787),.UNSPECIFIED.,.F.,.F.,(4,1,1,1,1,1,
1,4),(329.867228626928,330.775036298484,331.77439443205,332.773752565616,
333.773110699182,334.772468832748,335.771826966314,336.150413934108),
 .UNSPECIFIED.);
#629=B_SPLINE_CURVE_WITH_KNOTS('',3,(#27792,#27793,#27794,#27795,#27796,
#27797,#27798,#27799,#27800,#27801,#27802),.UNSPECIFIED.,.F.,.F.,(4,1,1,
1,1,1,1,1,4),(323.584043319749,323.808985448852,324.808343582418,325.807701715984,
326.80705984955,327.806417983116,328.805776116682,329.805134250248,329.867228626928),
 .UNSPECIFIED.);
#630=B_SPLINE_CURVE_WITH_KNOTS('',3,(#27803,#27804,#27805,#27806,#27807,
#27808,#27809,#27810,#27811,#27812,#27813),.UNSPECIFIED.,.F.,.F.,(4,1,1,
1,1,1,1,1,4),(323.584043319749,323.779529363522,324.778887497088,325.778245630654,
326.77760376422,327.776961897786,328.776320031352,329.775678164918,329.867228626928),
 .UNSPECIFIED.);
#631=B_SPLINE_CURVE_WITH_KNOTS('',3,(#27818,#27819,#27820,#27821,#27822,
#27823,#27824,#27825,#27826,#27827),.UNSPECIFIED.,.F.,.F.,(4,1,1,1,1,1,
1,4),(317.300858012569,317.812836647456,318.812194781022,319.811552914588,
320.810911048154,321.81026918172,322.809627315286,323.584043319749),
 .UNSPECIFIED.);
#632=B_SPLINE_CURVE_WITH_KNOTS('',3,(#27828,#27829,#27830,#27831,#27832,
#27833,#27834,#27835,#27836,#27837),.UNSPECIFIED.,.F.,.F.,(4,1,1,1,1,1,
1,4),(317.300858012569,317.783380562125,318.782738695691,319.782096829258,
320.781454962824,321.78081309639,322.780171229956,323.584043319749),
 .UNSPECIFIED.);
#633=B_SPLINE_CURVE_WITH_KNOTS('',3,(#27842,#27843,#27844,#27845,#27846,
#27847,#27848,#27849,#27850,#27851),.UNSPECIFIED.,.F.,.F.,(4,1,1,1,1,1,
1,4),(311.017672705389,311.816687846059,312.816045979625,313.815404113191,
314.814762246757,315.814120380323,316.81347851389,317.300858012569),
 .UNSPECIFIED.);
#634=B_SPLINE_CURVE_WITH_KNOTS('',3,(#27852,#27853,#27854,#27855,#27856,
#27857,#27858,#27859,#27860,#27861),.UNSPECIFIED.,.F.,.F.,(4,1,1,1,1,1,
1,4),(311.01767270539,311.787231760729,312.786589894295,313.785948027861,
314.785306161427,315.784664294993,316.784022428559,317.300858012569),
 .UNSPECIFIED.);
#635=B_SPLINE_CURVE_WITH_KNOTS('',3,(#27866,#27867,#27868,#27869,#27870,
#27871,#27872,#27873,#27874,#27875,#27876),.UNSPECIFIED.,.F.,.F.,(4,1,1,
1,1,1,1,1,4),(304.73448739821,304.821180911097,305.820539044663,306.819897178229,
307.819255311795,308.818613445361,309.817971578927,310.817329712493,311.017672705389),
 .UNSPECIFIED.);
#636=B_SPLINE_CURVE_WITH_KNOTS('',3,(#27877,#27878,#27879,#27880,#27881,
#27882,#27883,#27884,#27885,#27886,#27887),.UNSPECIFIED.,.F.,.F.,(4,1,1,
1,1,1,1,1,4),(304.73448739821,304.791724825767,305.791082959333,306.790441092899,
307.789799226465,308.789157360031,309.788515493597,310.787873627163,311.01767270539),
 .UNSPECIFIED.);
#637=B_SPLINE_CURVE_WITH_KNOTS('',3,(#27892,#27893,#27894,#27895,#27896,
#27897,#27898,#27899,#27900,#27901),.UNSPECIFIED.,.F.,.F.,(4,1,1,1,1,1,
1,4),(298.45130209103,298.825032109701,299.824390243267,300.823748376833,
301.823106510399,302.822464643965,303.821822777531,304.73448739821),
 .UNSPECIFIED.);
#638=B_SPLINE_CURVE_WITH_KNOTS('',3,(#27902,#27903,#27904,#27905,#27906,
#27907,#27908,#27909,#27910,#27911),.UNSPECIFIED.,.F.,.F.,(4,1,1,1,1,1,
1,4),(298.451302091031,298.795576024371,299.794934157937,300.794292291503,
301.793650425069,302.793008558635,303.792366692201,304.73448739821),
 .UNSPECIFIED.);
#639=B_SPLINE_CURVE_WITH_KNOTS('',3,(#27916,#27917,#27918,#27919,#27920,
#27921,#27922,#27923,#27924,#27925),.UNSPECIFIED.,.F.,.F.,(4,1,1,1,1,1,
1,4),(292.168116783851,292.828883308304,293.82824144187,294.827599575437,
295.826957709003,296.826315842569,297.825673976135,298.45130209103),
 .UNSPECIFIED.);
#640=B_SPLINE_CURVE_WITH_KNOTS('',3,(#27926,#27927,#27928,#27929,#27930,
#27931,#27932,#27933,#27934,#27935),.UNSPECIFIED.,.F.,.F.,(4,1,1,1,1,1,
1,4),(292.168116783851,292.799427222974,293.79878535654,294.798143490106,
295.797501623672,296.796859757238,297.796217890804,298.451302091031),
 .UNSPECIFIED.);
#641=B_SPLINE_CURVE_WITH_KNOTS('',3,(#27940,#27941,#27942,#27943,#27944,
#27945,#27946,#27947,#27948,#27949),.UNSPECIFIED.,.F.,.F.,(4,1,1,1,1,1,
1,4),(285.884931476671,286.832734506908,287.832092640474,288.83145077404,
289.830808907606,290.830167041172,291.829525174738,292.168116783851),
 .UNSPECIFIED.);
#642=B_SPLINE_CURVE_WITH_KNOTS('',3,(#27950,#27951,#27952,#27953,#27954,
#27955,#27956,#27957,#27958,#27959),.UNSPECIFIED.,.F.,.F.,(4,1,1,1,1,1,
1,4),(285.884931476672,286.803278421578,287.802636555144,288.80199468871,
289.801352822276,290.800710955842,291.800069089408,292.168116783851),
 .UNSPECIFIED.);
#643=B_SPLINE_CURVE_WITH_KNOTS('',3,(#27964,#27965,#27966,#27967,#27968,
#27969,#27970,#27971,#27972,#27973,#27974),.UNSPECIFIED.,.F.,.F.,(4,1,1,
1,1,1,1,1,4),(279.601746169492,279.837227571946,280.836585705512,281.835943839078,
282.835301972644,283.83466010621,284.834018239776,285.833376373342,285.884931476671),
 .UNSPECIFIED.);
#644=B_SPLINE_CURVE_WITH_KNOTS('',3,(#27975,#27976,#27977,#27978,#27979,
#27980,#27981,#27982,#27983,#27984,#27985),.UNSPECIFIED.,.F.,.F.,(4,1,1,
1,1,1,1,1,4),(279.601746169492,279.807771486616,280.807129620182,281.806487753748,
282.805845887314,283.80520402088,284.804562154446,285.803920288012,285.884931476672),
 .UNSPECIFIED.);
#645=B_SPLINE_CURVE_WITH_KNOTS('',3,(#27990,#27991,#27992,#27993,#27994,
#27995,#27996,#27997,#27998,#27999),.UNSPECIFIED.,.F.,.F.,(4,1,1,1,1,1,
1,4),(273.318560862312,273.84107877055,274.840436904116,275.839795037682,
276.839153171248,277.838511304814,278.83786943838,279.601746169492),
 .UNSPECIFIED.);
#646=B_SPLINE_CURVE_WITH_KNOTS('',3,(#28000,#28001,#28002,#28003,#28004,
#28005,#28006,#28007,#28008,#28009),.UNSPECIFIED.,.F.,.F.,(4,1,1,1,1,1,
1,4),(273.318560862312,273.811622685219,274.810980818785,275.810338952351,
276.809697085917,277.809055219484,278.80841335305,279.601746169492),
 .UNSPECIFIED.);
#647=B_SPLINE_CURVE_WITH_KNOTS('',3,(#28014,#28015,#28016,#28017,#28018,
#28019,#28020,#28021,#28022,#28023),.UNSPECIFIED.,.F.,.F.,(4,1,1,1,1,1,
1,4),(267.035375555133,267.844929969153,268.844288102719,269.843646236285,
270.843004369851,271.842362503417,272.841720636983,273.318560862312),
 .UNSPECIFIED.);
#648=B_SPLINE_CURVE_WITH_KNOTS('',3,(#28024,#28025,#28026,#28027,#28028,
#28029,#28030,#28031,#28032,#28033),.UNSPECIFIED.,.F.,.F.,(4,1,1,1,1,1,
1,4),(267.035375555133,267.815473883823,268.814832017389,269.814190150955,
270.813548284521,271.812906418087,272.812264551653,273.318560862312),
 .UNSPECIFIED.);
#649=B_SPLINE_CURVE_WITH_KNOTS('',3,(#28038,#28039,#28040,#28041,#28042,
#28043,#28044,#28045,#28046,#28047,#28048),.UNSPECIFIED.,.F.,.F.,(4,1,1,
1,1,1,1,1,4),(260.752190247953,260.849423034191,261.848781167757,262.848139301323,
263.847497434889,264.846855568455,265.846213702021,266.845571835587,267.035375555133),
 .UNSPECIFIED.);
#650=B_SPLINE_CURVE_WITH_KNOTS('',3,(#28049,#28050,#28051,#28052,#28053,
#28054,#28055,#28056,#28057,#28058,#28059),.UNSPECIFIED.,.F.,.F.,(4,1,1,
1,1,1,1,1,4),(260.752190247953,260.819966948861,261.819325082427,262.818683215993,
263.818041349559,264.817399483125,265.816757616691,266.816115750257,267.035375555133),
 .UNSPECIFIED.);
#651=B_SPLINE_CURVE_WITH_KNOTS('',3,(#28064,#28065,#28066,#28067,#28068,
#28069,#28070,#28071,#28072,#28073),.UNSPECIFIED.,.F.,.F.,(4,1,1,1,1,1,
1,4),(254.469004940773,254.853274232795,255.852632366361,256.851990499927,
257.851348633493,258.850706767059,259.850064900625,260.752190247953),
 .UNSPECIFIED.);
#652=B_SPLINE_CURVE_WITH_KNOTS('',3,(#28074,#28075,#28076,#28077,#28078,
#28079,#28080,#28081,#28082,#28083),.UNSPECIFIED.,.F.,.F.,(4,1,1,1,1,1,
1,4),(254.469004940774,254.823818147464,255.82317628103,256.822534414597,
257.821892548163,258.821250681729,259.820608815295,260.752190247953),
 .UNSPECIFIED.);
#653=B_SPLINE_CURVE_WITH_KNOTS('',3,(#28088,#28089,#28090,#28091,#28092,
#28093,#28094,#28095,#28096,#28097),.UNSPECIFIED.,.F.,.F.,(4,1,1,1,1,1,
1,4),(248.185819633594,248.857125431398,249.856483564964,250.85584169853,
251.855199832097,252.854557965663,253.853916099229,254.469004940773),
 .UNSPECIFIED.);
#654=B_SPLINE_CURVE_WITH_KNOTS('',3,(#28098,#28099,#28100,#28101,#28102,
#28103,#28104,#28105,#28106,#28107),.UNSPECIFIED.,.F.,.F.,(4,1,1,1,1,1,
1,4),(248.185819633594,248.827669346068,249.827027479634,250.8263856132,
251.825743746766,252.825101880332,253.824460013898,254.469004940774),
 .UNSPECIFIED.);
#655=B_SPLINE_CURVE_WITH_KNOTS('',3,(#28112,#28113,#28114,#28115,#28116,
#28117,#28118,#28119,#28120,#28121),.UNSPECIFIED.,.F.,.F.,(4,1,1,1,1,1,
1,4),(241.902634326414,242.860976630002,243.860334763568,244.859692897134,
245.8590510307,246.858409164266,247.857767297832,248.185819633594),
 .UNSPECIFIED.);
#656=B_SPLINE_CURVE_WITH_KNOTS('',3,(#28122,#28123,#28124,#28125,#28126,
#28127,#28128,#28129,#28130,#28131),.UNSPECIFIED.,.F.,.F.,(4,1,1,1,1,1,
1,4),(241.902634326415,242.831520544672,243.830878678238,244.830236811804,
245.82959494537,246.828953078936,247.828311212502,248.185819633594),
 .UNSPECIFIED.);
#657=B_SPLINE_CURVE_WITH_KNOTS('',3,(#28136,#28137,#28138,#28139,#28140,
#28141,#28142,#28143,#28144,#28145,#28146),.UNSPECIFIED.,.F.,.F.,(4,1,1,
1,1,1,1,1,4),(235.619449019235,235.86546969504,236.864827828606,237.864185962172,
238.863544095738,239.862902229304,240.86226036287,241.861618496436,241.902634326414),
 .UNSPECIFIED.);
#658=B_SPLINE_CURVE_WITH_KNOTS('',3,(#28147,#28148,#28149,#28150,#28151,
#28152,#28153,#28154,#28155,#28156,#28157),.UNSPECIFIED.,.F.,.F.,(4,1,1,
1,1,1,1,1,4),(235.619449019235,235.83601360971,236.835371743276,237.834729876842,
238.834088010408,239.833446143974,240.83280427754,241.832162411106,241.902634326415),
 .UNSPECIFIED.);
#659=B_SPLINE_CURVE_WITH_KNOTS('',3,(#28162,#28163,#28164,#28165,#28166,
#28167,#28168,#28169,#28170,#28171),.UNSPECIFIED.,.F.,.F.,(4,1,1,1,1,1,
1,4),(229.336263712055,229.869320893643,230.86867902721,231.868037160776,
232.867395294342,233.866753427908,234.866111561474,235.619449019235),
 .UNSPECIFIED.);
#660=B_SPLINE_CURVE_WITH_KNOTS('',3,(#28172,#28173,#28174,#28175,#28176,
#28177,#28178,#28179,#28180,#28181),.UNSPECIFIED.,.F.,.F.,(4,1,1,1,1,1,
1,4),(229.336263712055,229.839864808313,230.839222941879,231.838581075445,
232.837939209011,233.837297342577,234.836655476144,235.619449019235),
 .UNSPECIFIED.);
#661=B_SPLINE_CURVE_WITH_KNOTS('',3,(#28186,#28187,#28188,#28189,#28190,
#28191,#28192,#28193,#28194,#28195),.UNSPECIFIED.,.F.,.F.,(4,1,1,1,1,1,
1,4),(223.053078404876,223.873172092247,224.872530225813,225.871888359379,
226.871246492945,227.870604626511,228.869962760077,229.336263712055),
 .UNSPECIFIED.);
#662=B_SPLINE_CURVE_WITH_KNOTS('',3,(#28196,#28197,#28198,#28199,#28200,
#28201,#28202,#28203,#28204,#28205),.UNSPECIFIED.,.F.,.F.,(4,1,1,1,1,1,
1,4),(223.053078404876,223.843716006917,224.843074140483,225.842432274049,
226.841790407615,227.841148541181,228.840506674747,229.336263712055),
 .UNSPECIFIED.);
#663=B_SPLINE_CURVE_WITH_KNOTS('',3,(#28210,#28211,#28212,#28213,#28214,
#28215,#28216,#28217,#28218,#28219,#28220),.UNSPECIFIED.,.F.,.F.,(4,1,1,
1,1,1,1,1,4),(216.769893097696,216.877665157285,217.877023290851,218.876381424417,
219.875739557983,220.875097691549,221.874455825115,222.873813958681,223.053078404876),
 .UNSPECIFIED.);
#664=B_SPLINE_CURVE_WITH_KNOTS('',3,(#28221,#28222,#28223,#28224,#28225,
#28226,#28227,#28228,#28229,#28230,#28231),.UNSPECIFIED.,.F.,.F.,(4,1,1,
1,1,1,1,1,4),(216.769893097696,216.848209071955,217.847567205521,218.846925339087,
219.846283472653,220.845641606219,221.844999739785,222.844357873351,223.053078404876),
 .UNSPECIFIED.);
#665=B_SPLINE_CURVE_WITH_KNOTS('',3,(#28236,#28237,#28238,#28239,#28240,
#28241,#28242,#28243,#28244,#28245),.UNSPECIFIED.,.F.,.F.,(4,1,1,1,1,1,
1,4),(210.486707790516,210.881516355889,211.880874489455,212.880232623021,
213.879590756587,214.878948890153,215.878307023719,216.769893097696),
 .UNSPECIFIED.);
#666=B_SPLINE_CURVE_WITH_KNOTS('',3,(#28246,#28247,#28248,#28249,#28250,
#28251,#28252,#28253,#28254,#28255),.UNSPECIFIED.,.F.,.F.,(4,1,1,1,1,1,
1,4),(210.486707790517,210.852060270558,211.851418404124,212.85077653769,
213.850134671257,214.849492804823,215.848850938389,216.769893097696),
 .UNSPECIFIED.);
#667=B_SPLINE_CURVE_WITH_KNOTS('',3,(#28260,#28261,#28262,#28263,#28264,
#28265,#28266,#28267,#28268,#28269),.UNSPECIFIED.,.F.,.F.,(4,1,1,1,1,1,
1,4),(204.203522483337,204.885367554492,205.884725688058,206.884083821624,
207.88344195519,208.882800088756,209.882158222323,210.486707790516),
 .UNSPECIFIED.);
#668=B_SPLINE_CURVE_WITH_KNOTS('',3,(#28270,#28271,#28272,#28273,#28274,
#28275,#28276,#28277,#28278,#28279),.UNSPECIFIED.,.F.,.F.,(4,1,1,1,1,1,
1,4),(204.203522483337,204.855911469162,205.855269602728,206.854627736294,
207.85398586986,208.853344003426,209.852702136992,210.486707790517),
 .UNSPECIFIED.);
#669=B_SPLINE_CURVE_WITH_KNOTS('',3,(#28284,#28285,#28286,#28287,#28288,
#28289,#28290,#28291,#28292,#28293),.UNSPECIFIED.,.F.,.F.,(4,1,1,1,1,1,
1,4),(197.920337176157,198.889218753096,199.888576886662,200.887935020228,
201.887293153794,202.88665128736,203.886009420926,204.203522483337),
 .UNSPECIFIED.);
#670=B_SPLINE_CURVE_WITH_KNOTS('',3,(#28294,#28295,#28296,#28297,#28298,
#28299,#28300,#28301,#28302,#28303),.UNSPECIFIED.,.F.,.F.,(4,1,1,1,1,1,
1,4),(197.920337176158,198.859762667766,199.859120801332,200.858478934898,
201.857837068464,202.85719520203,203.856553335596,204.203522483337),
 .UNSPECIFIED.);
#671=B_SPLINE_CURVE_WITH_KNOTS('',3,(#28308,#28309,#28310,#28311,#28312,
#28313,#28314,#28315,#28316,#28317,#28318),.UNSPECIFIED.,.F.,.F.,(4,1,1,
1,1,1,1,1,4),(191.637151868978,191.893711818134,192.8930699517,193.892428085266,
194.891786218832,195.891144352398,196.890502485964,197.88986061953,197.920337176157),
 .UNSPECIFIED.);
#672=B_SPLINE_CURVE_WITH_KNOTS('',3,(#28319,#28320,#28321,#28322,#28323,
#28324,#28325,#28326,#28327,#28328,#28329),.UNSPECIFIED.,.F.,.F.,(4,1,1,
1,1,1,1,1,4),(191.637151868978,191.864255732803,192.86361386637,193.862971999936,
194.862330133502,195.861688267068,196.861046400634,197.8604045342,197.920337176158),
 .UNSPECIFIED.);
#673=B_SPLINE_CURVE_WITH_KNOTS('',3,(#28334,#28335,#28336,#28337,#28338,
#28339,#28340,#28341,#28342,#28343),.UNSPECIFIED.,.F.,.F.,(4,1,1,1,1,1,
1,4),(185.353966561798,185.897563016737,186.896921150303,187.89627928387,
188.895637417436,189.894995551002,190.894353684568,191.637151868978),
 .UNSPECIFIED.);
#674=B_SPLINE_CURVE_WITH_KNOTS('',3,(#28344,#28345,#28346,#28347,#28348,
#28349,#28350,#28351,#28352,#28353),.UNSPECIFIED.,.F.,.F.,(4,1,1,1,1,1,
1,4),(185.353966561799,185.868106931407,186.867465064973,187.866823198539,
188.866181332105,189.865539465671,190.864897599237,191.637151868978),
 .UNSPECIFIED.);
#675=B_SPLINE_CURVE_WITH_KNOTS('',3,(#28358,#28359,#28360,#28361,#28362,
#28363,#28364,#28365,#28366,#28367),.UNSPECIFIED.,.F.,.F.,(4,1,1,1,1,1,
1,4),(179.070781254619,179.901414215341,180.900772348907,181.900130482473,
182.899488616039,183.898846749605,184.898204883171,185.353966561798),
 .UNSPECIFIED.);
#676=B_SPLINE_CURVE_WITH_KNOTS('',3,(#28368,#28369,#28370,#28371,#28372,
#28373,#28374,#28375,#28376,#28377),.UNSPECIFIED.,.F.,.F.,(4,1,1,1,1,1,
1,4),(179.070781254619,179.871958130011,180.871316263577,181.870674397143,
182.870032530709,183.869390664275,184.868748797841,185.353966561799),
 .UNSPECIFIED.);
#677=B_SPLINE_CURVE_WITH_KNOTS('',3,(#28382,#28383,#28384,#28385,#28386,
#28387,#28388,#28389,#28390,#28391,#28392),.UNSPECIFIED.,.F.,.F.,(4,1,1,
1,1,1,1,1,4),(172.787595947439,172.905907280379,173.905265413945,174.904623547511,
175.903981681077,176.903339814643,177.902697948209,178.902056081775,179.070781254619),
 .UNSPECIFIED.);
#678=B_SPLINE_CURVE_WITH_KNOTS('',3,(#28393,#28394,#28395,#28396,#28397,
#28398,#28399,#28400,#28401,#28402,#28403),.UNSPECIFIED.,.F.,.F.,(4,1,1,
1,1,1,1,1,4),(172.787595947439,172.876451195049,173.875809328615,174.875167462181,
175.874525595747,176.873883729313,177.873241862879,178.872599996445,179.070781254619),
 .UNSPECIFIED.);
#679=B_SPLINE_CURVE_WITH_KNOTS('',3,(#28408,#28409,#28410,#28411,#28412,
#28413,#28414,#28415,#28416,#28417),.UNSPECIFIED.,.F.,.F.,(4,1,1,1,1,1,
1,4),(166.504410640259,166.909758478983,167.909116612549,168.908474746115,
169.907832879681,170.907191013247,171.906549146813,172.787595947439),
 .UNSPECIFIED.);
#680=B_SPLINE_CURVE_WITH_KNOTS('',3,(#28418,#28419,#28420,#28421,#28422,
#28423,#28424,#28425,#28426,#28427),.UNSPECIFIED.,.F.,.F.,(4,1,1,1,1,1,
1,4),(166.50441064026,166.880302393652,167.879660527218,168.879018660784,
169.87837679435,170.877734927916,171.877093061483,172.787595947439),
 .UNSPECIFIED.);
#681=B_SPLINE_CURVE_WITH_KNOTS('',3,(#28432,#28433,#28434,#28435,#28436,
#28437,#28438,#28439,#28440,#28441),.UNSPECIFIED.,.F.,.F.,(4,1,1,1,1,1,
1,4),(160.22122533308,160.913609677586,161.912967811152,162.912325944718,
163.911684078284,164.91104221185,165.910400345416,166.504410640259),
 .UNSPECIFIED.);
#682=B_SPLINE_CURVE_WITH_KNOTS('',3,(#28442,#28443,#28444,#28445,#28446,
#28447,#28448,#28449,#28450,#28451),.UNSPECIFIED.,.F.,.F.,(4,1,1,1,1,1,
1,4),(160.22122533308,160.884153592256,161.883511725822,162.882869859388,
163.882227992954,164.88158612652,165.880944260086,166.50441064026),
 .UNSPECIFIED.);
#683=B_SPLINE_CURVE_WITH_KNOTS('',3,(#28456,#28457,#28458,#28459,#28460,
#28461,#28462,#28463,#28464,#28465),.UNSPECIFIED.,.F.,.F.,(4,1,1,1,1,1,
1,4),(153.9380400259,154.91746087619,155.916819009756,156.916177143322,
157.915535276888,158.914893410454,159.91425154402,160.22122533308),
 .UNSPECIFIED.);
#684=B_SPLINE_CURVE_WITH_KNOTS('',3,(#28466,#28467,#28468,#28469,#28470,
#28471,#28472,#28473,#28474,#28475),.UNSPECIFIED.,.F.,.F.,(4,1,1,1,1,1,
1,4),(153.938040025901,154.88800479086,155.887362924426,156.886721057992,
157.886079191558,158.885437325124,159.88479545869,160.22122533308),
 .UNSPECIFIED.);
#685=B_SPLINE_CURVE_WITH_KNOTS('',3,(#28480,#28481,#28482,#28483,#28484,
#28485,#28486,#28487,#28488,#28489,#28490),.UNSPECIFIED.,.F.,.F.,(4,1,1,
1,1,1,1,1,4),(147.654854718721,147.921953941228,148.921312074794,149.92067020836,
150.920028341926,151.919386475492,152.918744609058,153.918102742624,153.9380400259),
 .UNSPECIFIED.);
#686=B_SPLINE_CURVE_WITH_KNOTS('',3,(#28491,#28492,#28493,#28494,#28495,
#28496,#28497,#28498,#28499,#28500,#28501),.UNSPECIFIED.,.F.,.F.,(4,1,1,
1,1,1,1,1,4),(147.654854718721,147.892497855897,148.891855989463,149.891214123029,
150.890572256596,151.889930390162,152.889288523728,153.888646657294,153.938040025901),
 .UNSPECIFIED.);
#687=B_SPLINE_CURVE_WITH_KNOTS('',3,(#28506,#28507,#28508,#28509,#28510,
#28511,#28512,#28513,#28514,#28515),.UNSPECIFIED.,.F.,.F.,(4,1,1,1,1,1,
1,4),(141.371669411541,141.925805139831,142.925163273397,143.924521406963,
144.92387954053,145.923237674096,146.922595807662,147.654854718721),
 .UNSPECIFIED.);
#688=B_SPLINE_CURVE_WITH_KNOTS('',3,(#28516,#28517,#28518,#28519,#28520,
#28521,#28522,#28523,#28524,#28525),.UNSPECIFIED.,.F.,.F.,(4,1,1,1,1,1,
1,4),(141.371669411542,141.896349054501,142.895707188067,143.895065321633,
144.894423455199,145.893781588765,146.893139722331,147.654854718721),
 .UNSPECIFIED.);
#689=B_SPLINE_CURVE_WITH_KNOTS('',3,(#28530,#28531,#28532,#28533,#28534,
#28535,#28536,#28537,#28538,#28539),.UNSPECIFIED.,.F.,.F.,(4,1,1,1,1,1,
1,4),(135.088484104362,135.929656338435,136.929014472001,137.928372605567,
138.927730739133,139.927088872699,140.926447006265,141.371669411541),
 .UNSPECIFIED.);
#690=B_SPLINE_CURVE_WITH_KNOTS('',3,(#28540,#28541,#28542,#28543,#28544,
#28545,#28546,#28547,#28548,#28549),.UNSPECIFIED.,.F.,.F.,(4,1,1,1,1,1,
1,4),(135.088484104362,135.900200253105,136.899558386671,137.898916520237,
138.898274653803,139.897632787369,140.896990920935,141.371669411542),
 .UNSPECIFIED.);
#691=B_SPLINE_CURVE_WITH_KNOTS('',3,(#28554,#28555,#28556,#28557,#28558,
#28559,#28560,#28561,#28562,#28563,#28564),.UNSPECIFIED.,.F.,.F.,(4,1,1,
1,1,1,1,1,4),(128.805298797182,128.934149403473,129.933507537039,130.932865670605,
131.932223804171,132.931581937737,133.930940071303,134.930298204869,135.088484104362),
 .UNSPECIFIED.);
#692=B_SPLINE_CURVE_WITH_KNOTS('',3,(#28565,#28566,#28567,#28568,#28569,
#28570,#28571,#28572,#28573,#28574,#28575),.UNSPECIFIED.,.F.,.F.,(4,1,1,
1,1,1,1,1,4),(128.805298797182,128.904693318142,129.904051451709,130.903409585275,
131.902767718841,132.902125852407,133.901483985973,134.900842119539,135.088484104362),
 .UNSPECIFIED.);
#693=B_SPLINE_CURVE_WITH_KNOTS('',3,(#28580,#28581,#28582,#28583,#28584,
#28585,#28586,#28587,#28588,#28589),.UNSPECIFIED.,.F.,.F.,(4,1,1,1,1,1,
1,4),(122.522113490002,122.938000602077,123.937358735643,124.936716869209,
125.936075002775,126.935433136341,127.934791269907,128.805298797182),
 .UNSPECIFIED.);
#694=B_SPLINE_CURVE_WITH_KNOTS('',3,(#28590,#28591,#28592,#28593,#28594,
#28595,#28596,#28597,#28598,#28599),.UNSPECIFIED.,.F.,.F.,(4,1,1,1,1,1,
1,4),(122.522113490003,122.908544516746,123.907902650312,124.907260783878,
125.906618917444,126.90597705101,127.905335184576,128.805298797182),
 .UNSPECIFIED.);
#695=B_SPLINE_CURVE_WITH_KNOTS('',3,(#28604,#28605,#28606,#28607,#28608,
#28609,#28610,#28611,#28612,#28613),.UNSPECIFIED.,.F.,.F.,(4,1,1,1,1,1,
1,4),(116.238928182823,116.94185180068,117.941209934246,118.940568067812,
119.939926201378,120.939284334944,121.93864246851,122.522113490002),
 .UNSPECIFIED.);
#696=B_SPLINE_CURVE_WITH_KNOTS('',3,(#28614,#28615,#28616,#28617,#28618,
#28619,#28620,#28621,#28622,#28623),.UNSPECIFIED.,.F.,.F.,(4,1,1,1,1,1,
1,4),(116.238928182823,116.91239571535,117.911753848916,118.911111982482,
119.910470116048,120.909828249614,121.90918638318,122.522113490003),
 .UNSPECIFIED.);
#697=B_SPLINE_CURVE_WITH_KNOTS('',3,(#28628,#28629,#28630,#28631,#28632,
#28633,#28634,#28635,#28636,#28637),.UNSPECIFIED.,.F.,.F.,(4,1,1,1,1,1,
1,4),(109.955742875643,110.945702999284,111.94506113285,112.944419266416,
113.943777399982,114.943135533548,115.942493667114,116.238928182823),
 .UNSPECIFIED.);
#698=B_SPLINE_CURVE_WITH_KNOTS('',3,(#28638,#28639,#28640,#28641,#28642,
#28643,#28644,#28645,#28646,#28647),.UNSPECIFIED.,.F.,.F.,(4,1,1,1,1,1,
1,4),(109.955742875644,110.916246913954,111.91560504752,112.914963181086,
113.914321314652,114.913679448218,115.913037581784,116.238928182823),
 .UNSPECIFIED.);
#699=B_SPLINE_CURVE_WITH_KNOTS('',3,(#28652,#28653,#28654,#28655,#28656,
#28657,#28658,#28659,#28660,#28661,#28662),.UNSPECIFIED.,.F.,.F.,(4,1,1,
1,1,1,1,1,4),(103.672557568464,103.950196064322,104.949554197888,105.948912331454,
106.94827046502,107.947628598586,108.946986732152,109.946344865718,109.955742875643),
 .UNSPECIFIED.);
#700=B_SPLINE_CURVE_WITH_KNOTS('',3,(#28663,#28664,#28665,#28666,#28667,
#28668,#28669,#28670,#28671,#28672,#28673),.UNSPECIFIED.,.F.,.F.,(4,1,1,
1,1,1,1,1,4),(103.672557568464,103.920739978991,104.920098112557,105.919456246123,
106.918814379689,107.918172513255,108.917530646822,109.916888780388,109.955742875644),
 .UNSPECIFIED.);
#701=B_SPLINE_CURVE_WITH_KNOTS('',3,(#28678,#28679,#28680,#28681,#28682,
#28683,#28684,#28685,#28686,#28687),.UNSPECIFIED.,.F.,.F.,(4,1,1,1,1,1,
1,4),(97.3893722612841,97.9540472629253,98.9534053964914,99.9527635300574,
100.952121663623,101.95147979719,102.950837930756,103.672557568464),
 .UNSPECIFIED.);
#702=B_SPLINE_CURVE_WITH_KNOTS('',3,(#28688,#28689,#28690,#28691,#28692,
#28693,#28694,#28695,#28696,#28697),.UNSPECIFIED.,.F.,.F.,(4,1,1,1,1,1,
1,4),(97.3893722612845,97.924591177595,98.9239493111611,99.9233074447271,
100.922665578293,101.922023711859,102.921381845425,103.672557568464),
 .UNSPECIFIED.);
#703=B_SPLINE_CURVE_WITH_KNOTS('',3,(#28702,#28703,#28704,#28705,#28706,
#28707,#28708,#28709,#28710,#28711),.UNSPECIFIED.,.F.,.F.,(4,1,1,1,1,1,
1,4),(91.1061869541045,91.9578984615291,92.9572565950951,93.9566147286612,
94.9559728622272,95.9553309957932,96.9546891293593,97.3893722612841),
 .UNSPECIFIED.);
#704=B_SPLINE_CURVE_WITH_KNOTS('',3,(#28712,#28713,#28714,#28715,#28716,
#28717,#28718,#28719,#28720,#28721),.UNSPECIFIED.,.F.,.F.,(4,1,1,1,1,1,
1,4),(91.1061869541048,91.9284423761987,92.9278005097648,93.9271586433308,
94.9265167768969,95.9258749104629,96.925233044029,97.3893722612845),
 .UNSPECIFIED.);
#705=B_SPLINE_CURVE_WITH_KNOTS('',3,(#28726,#28727,#28728,#28729,#28730,
#28731,#28732,#28733,#28734,#28735,#28736),.UNSPECIFIED.,.F.,.F.,(4,1,1,
1,1,1,1,1,4),(84.8230016469249,84.9623915265667,85.9617496601328,86.9611077936988,
87.9604659272649,88.9598240608309,89.959182194397,90.958540327963,91.1061869541045),
 .UNSPECIFIED.);
#706=B_SPLINE_CURVE_WITH_KNOTS('',3,(#28737,#28738,#28739,#28740,#28741,
#28742,#28743,#28744,#28745,#28746,#28747),.UNSPECIFIED.,.F.,.F.,(4,1,1,
1,1,1,1,1,4),(84.8230016469253,84.9329354412364,85.9322935748025,86.9316517083685,
87.9310098419346,88.9303679755006,89.9297261090666,90.9290842426327,91.1061869541048),
 .UNSPECIFIED.);
#707=B_SPLINE_CURVE_WITH_KNOTS('',3,(#28752,#28753,#28754,#28755,#28756,
#28757,#28758,#28759,#28760,#28761),.UNSPECIFIED.,.F.,.F.,(4,1,1,1,1,1,
1,4),(78.5398163397454,78.9662427251705,79.9656008587365,80.9649589923026,
81.9643171258686,82.9636752594347,83.9630333930007,84.8230016469249),
 .UNSPECIFIED.);
#708=B_SPLINE_CURVE_WITH_KNOTS('',3,(#28762,#28763,#28764,#28765,#28766,
#28767,#28768,#28769,#28770,#28771),.UNSPECIFIED.,.F.,.F.,(4,1,1,1,1,1,
1,4),(78.5398163397457,78.9367866398401,79.9361447734062,80.9355029069722,
81.9348610405383,82.9342191741043,83.9335773076704,84.8230016469253),
 .UNSPECIFIED.);
#709=B_SPLINE_CURVE_WITH_KNOTS('',3,(#28776,#28777,#28778,#28779,#28780,
#28781,#28782,#28783,#28784,#28785),.UNSPECIFIED.,.F.,.F.,(4,1,1,1,1,1,
1,4),(72.2566310325658,72.9700939237742,73.9694520573402,74.9688101909063,
75.9681683244723,76.9675264580384,77.9668845916044,78.5398163397454),
 .UNSPECIFIED.);
#710=B_SPLINE_CURVE_WITH_KNOTS('',3,(#28786,#28787,#28788,#28789,#28790,
#28791,#28792,#28793,#28794,#28795),.UNSPECIFIED.,.F.,.F.,(4,1,1,1,1,1,
1,4),(72.2566310325661,72.9406378384438,73.9399959720099,74.9393541055759,
75.938712239142,76.938070372708,77.9374285062741,78.5398163397457),
 .UNSPECIFIED.);
#711=B_SPLINE_CURVE_WITH_KNOTS('',3,(#28800,#28801,#28802,#28803,#28804,
#28805,#28806,#28807,#28808,#28809,#28810),.UNSPECIFIED.,.F.,.F.,(4,1,1,
1,1,1,1,1,4),(65.9734457253862,65.9745869888119,66.9739451223779,67.9733032559439,
68.97266138951,69.972019523076,70.9713776566421,71.9707357902081,72.2566310325658),
 .UNSPECIFIED.);
#712=B_SPLINE_CURVE_WITH_KNOTS('',3,(#28811,#28812,#28813,#28814,#28815,
#28816,#28817,#28818,#28819,#28820),.UNSPECIFIED.,.F.,.F.,(4,1,1,1,1,1,
1,4),(65.9734457253865,66.9444890370476,67.9438471706136,68.9432053041797,
69.9425634377457,70.9419215713118,71.9412797048778,72.2566310325661),
 .UNSPECIFIED.);
#713=B_SPLINE_CURVE_WITH_KNOTS('',3,(#28825,#28826,#28827,#28828,#28829,
#28830,#28831,#28832,#28833,#28834,#28835,#28836),.UNSPECIFIED.,.F.,.F.,
(4,1,1,1,1,1,1,1,1,4),(59.6902604182066,59.9784381874156,60.4781172541986,
60.9777963209816,61.4774753877646,61.9771544545477,62.9765125881137,63.9758707216798,
64.9752288552458,65.9734457253862),.UNSPECIFIED.);
#714=B_SPLINE_CURVE_WITH_KNOTS('',3,(#28837,#28838,#28839,#28840,#28841,
#28842,#28843,#28844,#28845,#28846,#28847),.UNSPECIFIED.,.F.,.F.,(4,1,1,
1,1,1,1,1,4),(59.6902604182069,59.9489821020852,60.9483402356513,61.9476983692173,
62.9470565027834,63.9464146363494,64.9457727699155,65.9451309034815,65.9734457253865),
 .UNSPECIFIED.);
#715=B_SPLINE_CURVE_WITH_KNOTS('',3,(#28852,#28853,#28854,#28855,#28856,
#28857,#28858,#28859,#28860,#28861,#28862,#28863,#28864,#28865,#28866,#28867,
#28868),.UNSPECIFIED.,.F.,.F.,(4,1,1,1,1,1,1,1,1,1,1,1,1,1,4),(53.407075111027,
53.4826103192363,53.9822893860193,54.4819684528023,54.9816475195853,55.4813265863684,
55.9810056531514,56.4806847199344,56.9803637867174,57.4800428535005,57.9797219202835,
58.4794009870665,58.9790800538495,59.4787591206325,59.6902604182066),
 .UNSPECIFIED.);
#716=B_SPLINE_CURVE_WITH_KNOTS('',3,(#28869,#28870,#28871,#28872,#28873,
#28874,#28875,#28876,#28877,#28878,#28879,#28880,#28881,#28882,#28883,#28884),
 .UNSPECIFIED.,.F.,.F.,(4,1,1,1,1,1,1,1,1,1,1,1,1,4),(53.4070751110273,
53.4531542339059,53.9528333006889,54.452512367472,54.952191434255,55.451870501038,
55.951549567821,56.4512286346041,56.9509077013871,57.4505867681701,57.9502658349531,
58.4499449017362,58.9496239685192,59.6902604182069),.UNSPECIFIED.);
#717=B_SPLINE_CURVE_WITH_KNOTS('',3,(#28889,#28890,#28891,#28892,#28893,
#28894,#28895,#28896,#28897,#28898,#28899,#28900,#28901,#28902,#28903,#28904),
 .UNSPECIFIED.,.F.,.F.,(4,1,1,1,1,1,1,1,1,1,1,1,1,4),(47.1238898038474,
47.48646151784,47.986140584623,48.485819651406,48.9854987181891,49.4851777849721,
49.9848568517551,50.4845359185381,50.9842149853212,51.4838940521042,51.9835731188872,
52.4832521856702,52.9829312524532,53.407075111027),.UNSPECIFIED.);
#718=B_SPLINE_CURVE_WITH_KNOTS('',3,(#28905,#28906,#28907,#28908,#28909,
#28910,#28911,#28912,#28913,#28914,#28915,#28916,#28917,#28918,#28919,#28920),
 .UNSPECIFIED.,.F.,.F.,(4,1,1,1,1,1,1,1,1,1,1,1,1,4),(47.1238898038477,
47.4570054325096,47.9566844992927,48.4563635660757,48.9560426328587,49.4557216996417,
49.9554007664248,50.4550798332078,50.9547588999908,51.4544379667738,51.9541170335568,
52.4537961003399,52.9534751671229,53.4070751110273),.UNSPECIFIED.);
#719=B_SPLINE_CURVE_WITH_KNOTS('',3,(#28925,#28926,#28927,#28928,#28929,
#28930,#28931,#28932,#28933,#28934,#28935,#28936,#28937,#28938,#28939,#28940,
#28941),.UNSPECIFIED.,.F.,.F.,(4,1,1,1,1,1,1,1,1,1,1,1,1,1,4),(40.8407044966678,
40.9906336496607,41.4903127164437,41.9899917832267,42.4896708500098,42.9893499167928,
43.4890289835758,43.9887080503588,44.4883871171419,44.9880661839249,45.4877452507079,
45.9874243174909,46.4871033842739,46.986782451057,47.1238898038474),
 .UNSPECIFIED.);
#720=B_SPLINE_CURVE_WITH_KNOTS('',3,(#28942,#28943,#28944,#28945,#28946,
#28947,#28948,#28949,#28950,#28951,#28952,#28953,#28954,#28955,#28956,#28957,
#28958),.UNSPECIFIED.,.F.,.F.,(4,1,1,1,1,1,1,1,1,1,1,1,1,1,4),(40.8407044966681,
40.9611775643303,41.4608566311134,41.9605356978964,42.4602147646794,42.9598938314624,
43.4595728982454,43.9592519650285,44.4589310318115,44.9586100985945,45.4582891653775,
45.9579682321606,46.4576472989436,46.9573263657266,47.1238898038477),
 .UNSPECIFIED.);
#721=B_SPLINE_CURVE_WITH_KNOTS('',3,(#28963,#28964,#28965,#28966,#28967,
#28968,#28969,#28970,#28971,#28972,#28973,#28974,#28975,#28976,#28977,#28978),
 .UNSPECIFIED.,.F.,.F.,(4,1,1,1,1,1,1,1,1,1,1,1,1,4),(34.5575191894882,
34.9944848482644,35.4941639150474,35.9938429818305,36.4935220486135,36.9932011153965,
37.4928801821795,37.9925592489626,38.4922383157456,38.9919173825286,39.4915964493116,
39.9912755160946,40.4909545828777,40.8407044966678),.UNSPECIFIED.);
#722=B_SPLINE_CURVE_WITH_KNOTS('',3,(#28979,#28980,#28981,#28982,#28983,
#28984,#28985,#28986,#28987,#28988,#28989,#28990,#28991,#28992,#28993,#28994),
 .UNSPECIFIED.,.F.,.F.,(4,1,1,1,1,1,1,1,1,1,1,1,1,4),(34.5575191894886,
34.965028762934,35.4647078297171,35.9643868965001,36.4640659632831,36.9637450300661,
37.4634240968492,37.9631031636322,38.4627822304152,38.9624612971982,39.4621403639813,
39.9618194307643,40.4614984975473,40.8407044966681),.UNSPECIFIED.);
#723=B_SPLINE_CURVE_WITH_KNOTS('',3,(#28999,#29000,#29001,#29002,#29003,
#29004,#29005,#29006,#29007,#29008,#29009,#29010,#29011,#29012,#29013,#29014,
#29015),.UNSPECIFIED.,.F.,.F.,(4,1,1,1,1,1,1,1,1,1,1,1,1,1,4),(28.2743338823086,
28.4986569800851,28.9983360468681,29.4980151136512,29.9976941804342,30.4973732472172,
30.9970523140002,31.4967313807832,31.9964104475663,32.4960895143493,32.9957685811323,
33.4954476479153,33.9951267146984,34.4948057814814,34.5575191894882),
 .UNSPECIFIED.);
#724=B_SPLINE_CURVE_WITH_KNOTS('',3,(#29016,#29017,#29018,#29019,#29020,
#29021,#29022,#29023,#29024,#29025,#29026,#29027,#29028,#29029,#29030,#29031,
#29032),.UNSPECIFIED.,.F.,.F.,(4,1,1,1,1,1,1,1,1,1,1,1,1,1,4),(28.2743338823089,
28.4692008947547,28.9688799615378,29.4685590283208,29.9682380951038,30.4679171618868,
30.9675962286699,31.4672752954529,31.9669543622359,32.4666334290189,32.966312495802,
33.465991562585,33.965670629368,34.465349696151,34.5575191894886),
 .UNSPECIFIED.);
#725=B_SPLINE_CURVE_WITH_KNOTS('',3,(#29037,#29038,#29039,#29040,#29041,
#29042,#29043,#29044,#29045,#29046,#29047,#29048,#29049,#29050,#29051,#29052,
#29053),.UNSPECIFIED.,.F.,.F.,(4,1,1,1,1,1,1,1,1,1,1,1,1,1,4),(21.991148575129,
22.0028291119058,22.5025081786888,23.0021872454719,23.5018663122549,24.0015453790379,
24.5012244458209,25.0009035126039,25.500582579387,26.00026164617,26.499940712953,
26.999619779736,27.4992988465191,27.9989779133021,28.2743338823086),
 .UNSPECIFIED.);
#726=B_SPLINE_CURVE_WITH_KNOTS('',3,(#29054,#29055,#29056,#29057,#29058,
#29059,#29060,#29061,#29062,#29063,#29064,#29065,#29066,#29067,#29068,#29069),
 .UNSPECIFIED.,.F.,.F.,(4,1,1,1,1,1,1,1,1,1,1,1,1,4),(21.9911485751294,
22.4730520933585,22.9727311601415,23.4724102269245,23.9720892937075,24.4717683604905,
24.9714474272736,25.4711264940566,25.9708055608396,26.4704846276226,26.9701636944057,
27.4698427611887,27.9695218279717,28.2743338823089),.UNSPECIFIED.);
#727=B_SPLINE_CURVE_WITH_KNOTS('',3,(#29074,#29075,#29076,#29077,#29078,
#29079,#29080,#29081,#29082,#29083,#29084,#29085,#29086,#29087,#29088,#29089),
 .UNSPECIFIED.,.F.,.F.,(4,1,1,1,1,1,1,1,1,1,1,1,1,4),(15.7079632679495,
16.0066803105095,16.5063593772925,17.0060384440756,17.5057175108586,18.0053965776416,
18.5050756444246,19.0047547112077,19.5044337779907,20.0041128447737,20.5037919115567,
21.0034709783398,21.5031500451228,21.991148575129),.UNSPECIFIED.);
#728=B_SPLINE_CURVE_WITH_KNOTS('',3,(#29090,#29091,#29092,#29093,#29094,
#29095,#29096,#29097,#29098,#29099,#29100,#29101,#29102,#29103,#29104,#29105,
#29106),.UNSPECIFIED.,.F.,.F.,(4,1,1,1,1,1,1,1,1,1,1,1,1,1,4),(15.7079632679498,
15.9772242251791,16.4769032919622,16.9765823587452,17.4762614255282,17.9759404923112,
18.4756195590943,18.9752986258773,19.4749776926603,19.9746567594433,20.4743358262264,
20.9740148930094,21.4736939597924,21.9733730265754,21.9911485751294),
 .UNSPECIFIED.);
#729=B_SPLINE_CURVE_WITH_KNOTS('',3,(#29111,#29112,#29113,#29114,#29115,
#29116,#29117,#29118,#29119,#29120,#29121,#29122,#29123,#29124,#29125,#29126,
#29127,#29128,#29129,#29130,#29131,#29132,#29133,#29134,#29135,#29136,#29137,
#29138,#29139,#29140,#29141,#29142,#29143,#29144,#29145,#29146,#29147),
 .UNSPECIFIED.,.F.,.F.,(4,3,3,3,3,3,3,3,3,3,3,3,4),(0.,0.000373494560508806,
0.0620760815771024,0.112839239637108,0.153038169722591,0.175804963675793,
0.247183842626883,0.319084136954533,0.344742425233931,0.363606980156396,
0.439518700737557,0.51795432283266,0.534785019937482),.UNSPECIFIED.);
#730=B_SPLINE_CURVE_WITH_KNOTS('',3,(#29149,#29150,#29151,#29152,#29153,
#29154,#29155,#29156,#29157,#29158,#29159,#29160,#29161,#29162,#29163,#29164,
#29165,#29166,#29167,#29168,#29169,#29170,#29171,#29172,#29173,#29174,#29175,
#29176,#29177,#29178,#29179,#29180,#29181,#29182,#29183,#29184,#29185),
 .UNSPECIFIED.,.F.,.F.,(4,3,3,3,3,3,3,3,3,3,3,3,4),(0.,0.000511892384038064,
0.078754853834616,0.155070466132989,0.20164291816609,0.227017770490094,
0.290460834304131,0.352619921814331,0.383703668213755,0.403796492255862,
0.466621120797767,0.52704524650008,0.539097184344933),.UNSPECIFIED.);
#731=B_SPLINE_CURVE_WITH_KNOTS('',3,(#31185,#31186,#31187,#31188,#31189,
#31190,#31191,#31192,#31193,#31194,#31195,#31196,#31197,#31198,#31199,#31200,
#31201,#31202,#31203,#31204,#31205,#31206,#31207,#31208,#31209,#31210,#31211,
#31212,#31213,#31214,#31215,#31216,#31217,#31218,#31219,#31220,#31221,#31222,
#31223,#31224),.UNSPECIFIED.,.F.,.F.,(4,3,3,3,3,3,3,3,3,3,3,3,3,4),(-0.53478501993692,
-0.534277081309421,-0.456439695901019,-0.38064245929011,-0.348102919117109,
-0.328886681298388,-0.258595553176405,-0.246742105655551,-0.185056579241663,
-0.163339235199672,-0.143463957830519,-0.0808484674142256,-0.0206857924044652,
0.),.UNSPECIFIED.);
#732=B_SPLINE_CURVE_WITH_KNOTS('',3,(#31225,#31226,#31227,#31228,#31229,
#31230,#31231,#31232,#31233,#31234,#31235,#31236,#31237,#31238,#31239,#31240,
#31241,#31242,#31243,#31244,#31245,#31246,#31247,#31248,#31249),
 .UNSPECIFIED.,.F.,.F.,(4,3,3,3,3,3,3,3,4),(390.000549715688,390.249351157541,
390.749030224325,391.248709291108,391.748388357891,392.248067424674,392.747746491457,
393.24742555824,393.746279249921),.UNSPECIFIED.);
#733=B_SPLINE_CURVE_WITH_KNOTS('',3,(#31250,#31251,#31252,#31253,#31254,
#31255,#31256,#31257,#31258,#31259,#31260,#31261,#31262,#31263,#31264),
 .UNSPECIFIED.,.F.,.F.,(4,1,1,1,1,1,1,1,1,1,1,1,4),(9.98190079888485,10.4807544905659,
10.9804335573489,11.4801126241319,11.979791690915,12.479470757698,12.979149824481,
13.478828891264,13.9785079580471,14.4781870248301,14.9778660916131,15.4775451583961,
15.7079632679498),.UNSPECIFIED.);
#734=B_SPLINE_CURVE_WITH_KNOTS('',3,(#31266,#31267,#31268,#31269,#31270,
#31271,#31272,#31273,#31274,#31275,#31276),.UNSPECIFIED.,.F.,.F.,(4,1,1,
1,1,1,1,1,4),(12.0092477762453,12.5089268430284,13.0086059098114,13.5082849765944,
14.0079640433774,14.5076431101605,15.0073221769435,15.5070012437265,15.7079632679495),
 .UNSPECIFIED.);
#735=B_SPLINE_CURVE_WITH_KNOTS('',3,(#33270,#33271,#33272,#33273,#33274,
#33275,#33276,#33277,#33278,#33279,#33280,#33281,#33282,#33283,#33284,#33285,
#33286,#33287,#33288,#33289,#33290,#33291,#33292,#33293,#33294,#33295,#33296,
#33297,#33298,#33299,#33300,#33301,#33302,#33303,#33304,#33305,#33306,#33307,
#33308,#33309),.UNSPECIFIED.,.F.,.F.,(4,3,3,3,3,3,3,3,3,3,3,3,3,4),(-0.539097184344981,
-0.538720824057998,-0.476544551511477,-0.429912347101587,-0.401091234701428,
-0.381803774975435,-0.313681369269712,-0.290015733871917,-0.24230273417063,
-0.214804629165427,-0.192593514291413,-0.116696500404398,-0.0381316372362206,
0.),.UNSPECIFIED.);
#736=B_SPLINE_CURVE_WITH_KNOTS('',3,(#33310,#33311,#33312,#33313,#33314,
#33315,#33316,#33317,#33318,#33319),.UNSPECIFIED.,.F.,.F.,(4,3,3,4),(-394.746462758588,
-394.246783691805,-393.747104625022,-393.256204536838),.UNSPECIFIED.);
#737=B_SPLINE_CURVE_WITH_KNOTS('',3,(#33386,#33387,#33388,#33389,#33390,
#33391,#33392,#33393),.UNSPECIFIED.,.F.,.F.,(4,2,2,4),(0.756005737987019,
0.793568827564653,0.872922520054208,0.952276212543762),.UNSPECIFIED.);
#738=B_SPLINE_CURVE_WITH_KNOTS('',3,(#33396,#33397,#33398,#33399,#33400,
#33401,#33402,#33403,#33404,#33405,#33406,#33407,#33408,#33409),
 .UNSPECIFIED.,.F.,.F.,(4,2,2,2,2,2,4),(0.121154929624509,0.158718019202145,
0.238071711691699,0.317425404181254,0.396779096670809,0.476132789160363,
0.513695878738001),.UNSPECIFIED.);
#739=B_SPLINE_CURVE_WITH_KNOTS('',3,(#33410,#33411,#33412,#33413,#33414,
#33415,#33416,#33417),.UNSPECIFIED.,.F.,.F.,(4,2,2,4),(0.952276212543762,
1.03162990503332,1.11098359752287,1.14854668710052),.UNSPECIFIED.);
#740=B_SPLINE_CURVE_WITH_KNOTS('',3,(#33421,#33422,#33423,#33424,#33425,
#33426,#33427,#33428,#33429,#33430),.UNSPECIFIED.,.F.,.F.,(4,2,2,2,4),(0.,
0.0792165807733642,0.158433161546728,0.237648697074572,0.316864232602417),
 .UNSPECIFIED.);
#741=B_SPLINE_CURVE_WITH_KNOTS('',3,(#33431,#33432,#33433,#33434,#33435,
#33436,#33437,#33438,#33439,#33440,#33441,#33442,#33443,#33444,#33445,#33446,
#33447,#33448,#33449,#33450,#33451,#33452,#33453,#33454,#33455,#33456),
 .UNSPECIFIED.,.F.,.F.,(4,2,2,2,2,2,2,2,2,2,2,2,4),(0.316864232602417,0.396079768130261,
0.475295303658105,0.554511884431469,0.633728465204833,0.712945045978197,
0.792161626751562,0.871377162279406,0.95059269780725,1.02980823333509,1.10902376886294,
1.1882403496363,1.26745693040967),.UNSPECIFIED.);
#742=B_SPLINE_CURVE_WITH_KNOTS('',3,(#33488,#33489,#33490,#33491,#33492,
#33493),.UNSPECIFIED.,.F.,.F.,(4,2,4),(0.803821788694078,0.872950991853625,
0.952307212900975),.UNSPECIFIED.);
#743=B_SPLINE_CURVE_WITH_KNOTS('',3,(#33496,#33497,#33498,#33499,#33500,
#33501,#33502,#33503,#33504,#33505),.UNSPECIFIED.,.F.,.F.,(4,2,2,2,4),(0.168950313426762,
0.238079516586309,0.317435737633658,0.396791958681008,0.465921161840561),
 .UNSPECIFIED.);
#744=B_SPLINE_CURVE_WITH_KNOTS('',3,(#33506,#33507,#33508,#33509,#33510,
#33511),.UNSPECIFIED.,.F.,.F.,(4,2,4),(0.952307212900975,1.03166343394832,
1.10079263710787),.UNSPECIFIED.);
#745=B_SPLINE_CURVE_WITH_KNOTS('',3,(#33515,#33516,#33517,#33518,#33519,
#33520,#33521,#33522,#33523,#33524),.UNSPECIFIED.,.F.,.F.,(4,2,2,2,4),(0.,
0.0792165807733642,0.158433161546728,0.237648697074572,0.316864232602417),
 .UNSPECIFIED.);
#746=B_SPLINE_CURVE_WITH_KNOTS('',3,(#33525,#33526,#33527,#33528,#33529,
#33530,#33531,#33532,#33533,#33534,#33535,#33536,#33537,#33538,#33539,#33540,
#33541,#33542,#33543,#33544,#33545,#33546,#33547,#33548,#33549,#33550),
 .UNSPECIFIED.,.F.,.F.,(4,2,2,2,2,2,2,2,2,2,2,2,4),(0.316864232602417,0.396079768130261,
0.475295303658105,0.554511884431469,0.633728465204833,0.712945045978197,
0.792161626751562,0.871377162279406,0.95059269780725,1.02980823333509,1.10902376886294,
1.1882403496363,1.26745693040967),.UNSPECIFIED.);
#747=SPHERICAL_SURFACE('',#13913,0.29765);
#748=SPHERICAL_SURFACE('',#13915,0.29765);
#749=SPHERICAL_SURFACE('',#13917,0.29765);
#750=SPHERICAL_SURFACE('',#13919,0.29765);
#751=SPHERICAL_SURFACE('',#13921,0.29765);
#752=SPHERICAL_SURFACE('',#13923,0.29765);
#753=SPHERICAL_SURFACE('',#13925,0.29765);
#754=SPHERICAL_SURFACE('',#13928,0.309556);
#755=SPHERICAL_SURFACE('',#13944,0.309556);
#756=SPHERICAL_SURFACE('',#13949,0.309556);
#757=SPHERICAL_SURFACE('',#13955,0.309556);
#758=SPHERICAL_SURFACE('',#13960,0.309556);
#759=SPHERICAL_SURFACE('',#13965,0.309556);
#760=SPHERICAL_SURFACE('',#13973,0.309556);
#761=SPHERICAL_SURFACE('',#14041,0.3969);
#762=SPHERICAL_SURFACE('',#14043,0.3969);
#763=SPHERICAL_SURFACE('',#14045,0.3969);
#764=SPHERICAL_SURFACE('',#14047,0.3969);
#765=SPHERICAL_SURFACE('',#14049,0.3969);
#766=SPHERICAL_SURFACE('',#14051,0.3969);
#767=SPHERICAL_SURFACE('',#14053,0.3969);
#768=SPHERICAL_SURFACE('',#14055,0.3969);
#769=SPHERICAL_SURFACE('',#14058,0.412776);
#770=SPHERICAL_SURFACE('',#14074,0.412776);
#771=SPHERICAL_SURFACE('',#14079,0.412776);
#772=SPHERICAL_SURFACE('',#14084,0.412776);
#773=SPHERICAL_SURFACE('',#14089,0.412776);
#774=SPHERICAL_SURFACE('',#14094,0.412776);
#775=SPHERICAL_SURFACE('',#14099,0.412776);
#776=SPHERICAL_SURFACE('',#14107,0.412776);
#777=CONICAL_SURFACE('',#13884,0.63,0.785398163397448);
#778=CONICAL_SURFACE('',#13891,0.63,0.785398163397448);
#779=CONICAL_SURFACE('',#13904,1.57,0.785398163397449);
#780=CONICAL_SURFACE('',#13908,1.57,0.785398163397449);
#781=CONICAL_SURFACE('',#14012,1.05,0.785398163397449);
#782=CONICAL_SURFACE('',#14019,1.05,0.785398163397449);
#783=CONICAL_SURFACE('',#14032,2.3,0.785398163397449);
#784=CONICAL_SURFACE('',#14036,2.3,0.785398163397449);
#785=CONICAL_SURFACE('',#14201,0.275,0.785398163397449);
#786=CONICAL_SURFACE('',#14224,0.4,0.785398163397448);
#787=CONICAL_SURFACE('',#14228,0.41,0.785398163397448);
#788=CONICAL_SURFACE('',#14232,0.26,0.463647609000806);
#789=CONICAL_SURFACE('',#14390,0.275,0.785398163397449);
#790=CONICAL_SURFACE('',#14417,0.4,0.785398163397448);
#791=CONICAL_SURFACE('',#14421,0.41,0.785398163397448);
#792=CONICAL_SURFACE('',#14425,0.26,0.463647609000806);
#793=CONICAL_SURFACE('',#14476,0.325,0.785398163397448);
#794=CONICAL_SURFACE('',#14480,0.335,0.785398163397448);
#795=CONICAL_SURFACE('',#14484,0.21,0.463647609000806);
#796=CONICAL_SURFACE('',#14488,0.18,0.785398163397448);
#797=CONICAL_SURFACE('',#14502,0.4,0.785398163397448);
#798=CONICAL_SURFACE('',#14506,0.41,0.785398163397448);
#799=CONICAL_SURFACE('',#14510,0.26,0.463647609000806);
#800=CONICAL_SURFACE('',#14514,0.225,0.785398163397448);
#801=CONICAL_SURFACE('',#14787,0.235,0.785398163397448);
#802=CONICAL_SURFACE('',#14791,0.2125,0.785398163397448);
#803=CONICAL_SURFACE('',#14806,0.475,0.785398163397449);
#804=CONICAL_SURFACE('',#14810,0.485,0.785398163397448);
#805=CONICAL_SURFACE('',#14814,0.31,0.463647609000806);
#806=CONICAL_SURFACE('',#14818,0.27,0.785398163397448);
#807=TOROIDAL_SURFACE('',#13873,1.1,0.309556);
#808=TOROIDAL_SURFACE('',#13893,1.1,0.309556);
#809=TOROIDAL_SURFACE('',#14001,1.675,0.412776);
#810=TOROIDAL_SURFACE('',#14021,1.675,0.412776);
#811=SHAPE_REPRESENTATION_RELATIONSHIP('SRR','None',#34184,#855);
#812=SHAPE_REPRESENTATION_RELATIONSHIP('SRR','None',#34185,#856);
#813=SHAPE_REPRESENTATION_RELATIONSHIP('SRR','None',#34186,#857);
#814=SHAPE_REPRESENTATION_RELATIONSHIP('SRR','None',#34187,#858);
#815=SHAPE_REPRESENTATION_RELATIONSHIP('SRR','None',#34188,#859);
#816=SHAPE_REPRESENTATION_RELATIONSHIP('SRR','None',#34189,#860);
#817=SHAPE_REPRESENTATION_RELATIONSHIP('SRR','None',#34190,#861);
#818=SHAPE_REPRESENTATION_RELATIONSHIP('SRR','None',#34191,#862);
#819=SHAPE_REPRESENTATION_RELATIONSHIP('SRR','None',#34192,#863);
#820=SHAPE_REPRESENTATION_RELATIONSHIP('SRR','None',#34194,#864);
#821=SHAPE_REPRESENTATION_RELATIONSHIP('SRR','None',#34195,#865);
#822=SHAPE_REPRESENTATION_RELATIONSHIP('SRR','None',#34196,#866);
#823=SHAPE_REPRESENTATION_RELATIONSHIP('SRR','None',#34197,#867);
#824=SHAPE_REPRESENTATION_RELATIONSHIP('SRR','None',#34198,#868);
#825=SHAPE_REPRESENTATION_RELATIONSHIP('SRR','None',#34200,#869);
#826=SHAPE_REPRESENTATION_RELATIONSHIP('SRR','None',#34201,#870);
#827=SHAPE_REPRESENTATION_RELATIONSHIP('SRR','None',#34202,#871);
#828=SHAPE_REPRESENTATION_RELATIONSHIP('SRR','None',#34203,#872);
#829=SHAPE_REPRESENTATION_RELATIONSHIP('SRR','None',#34204,#873);
#830=SHAPE_REPRESENTATION_RELATIONSHIP('SRR','None',#34205,#874);
#831=SHAPE_REPRESENTATION_RELATIONSHIP('SRR','None',#34206,#875);
#832=SHAPE_REPRESENTATION_RELATIONSHIP('SRR','None',#34207,#876);
#833=SHAPE_REPRESENTATION_RELATIONSHIP('SRR','None',#34208,#877);
#834=SHAPE_REPRESENTATION_RELATIONSHIP('SRR','None',#34210,#878);
#835=SHAPE_REPRESENTATION_RELATIONSHIP('SRR','None',#34211,#879);
#836=SHAPE_REPRESENTATION_RELATIONSHIP('SRR','None',#34212,#880);
#837=SHAPE_REPRESENTATION_RELATIONSHIP('SRR','None',#34214,#881);
#838=SHAPE_REPRESENTATION_RELATIONSHIP('SRR','None',#34215,#882);
#839=SHAPE_REPRESENTATION_RELATIONSHIP('SRR','None',#34216,#883);
#840=SHAPE_REPRESENTATION_RELATIONSHIP('SRR','None',#34217,#884);
#841=SHAPE_REPRESENTATION_RELATIONSHIP('SRR','None',#34218,#885);
#842=SHAPE_REPRESENTATION_RELATIONSHIP('SRR','None',#34219,#886);
#843=SHAPE_REPRESENTATION_RELATIONSHIP('SRR','None',#34220,#887);
#844=SHAPE_REPRESENTATION_RELATIONSHIP('SRR','None',#34221,#888);
#845=SHAPE_REPRESENTATION_RELATIONSHIP('SRR','None',#34223,#889);
#846=SHAPE_REPRESENTATION_RELATIONSHIP('SRR','None',#34224,#890);
#847=SHAPE_REPRESENTATION_RELATIONSHIP('SRR','None',#34225,#891);
#848=SHAPE_REPRESENTATION_RELATIONSHIP('SRR','None',#34226,#892);
#849=SHAPE_REPRESENTATION_RELATIONSHIP('SRR','None',#34227,#893);
#850=SHAPE_REPRESENTATION_RELATIONSHIP('SRR','None',#34228,#894);
#851=SHAPE_REPRESENTATION_RELATIONSHIP('SRR','None',#34229,#895);
#852=SHAPE_REPRESENTATION_RELATIONSHIP('SRR','None',#34230,#896);
#853=SHAPE_REPRESENTATION_RELATIONSHIP('SRR','None',#34231,#897);
#854=SHAPE_REPRESENTATION_RELATIONSHIP('SRR','None',#34232,#898);
#855=ADVANCED_BREP_SHAPE_REPRESENTATION('',(#958),#33932);
#856=ADVANCED_BREP_SHAPE_REPRESENTATION('',(#959),#33933);
#857=ADVANCED_BREP_SHAPE_REPRESENTATION('',(#960),#33934);
#858=ADVANCED_BREP_SHAPE_REPRESENTATION('',(#961),#33935);
#859=ADVANCED_BREP_SHAPE_REPRESENTATION('',(#962),#33936);
#860=ADVANCED_BREP_SHAPE_REPRESENTATION('',(#963),#33937);
#861=ADVANCED_BREP_SHAPE_REPRESENTATION('',(#964),#33938);
#862=ADVANCED_BREP_SHAPE_REPRESENTATION('',(#965),#33939);
#863=ADVANCED_BREP_SHAPE_REPRESENTATION('',(#966),#33940);
#864=ADVANCED_BREP_SHAPE_REPRESENTATION('',(#967),#33942);
#865=ADVANCED_BREP_SHAPE_REPRESENTATION('',(#968),#33943);
#866=ADVANCED_BREP_SHAPE_REPRESENTATION('',(#969,#970,#971,#972,#973,#974,
#975),#33944);
#867=ADVANCED_BREP_SHAPE_REPRESENTATION('',(#976),#33945);
#868=ADVANCED_BREP_SHAPE_REPRESENTATION('',(#977,#978),#33946);
#869=ADVANCED_BREP_SHAPE_REPRESENTATION('',(#979),#33948);
#870=ADVANCED_BREP_SHAPE_REPRESENTATION('',(#980),#33949);
#871=ADVANCED_BREP_SHAPE_REPRESENTATION('',(#981,#982,#983,#984,#985,#986,
#987,#988),#33950);
#872=ADVANCED_BREP_SHAPE_REPRESENTATION('',(#989),#33951);
#873=ADVANCED_BREP_SHAPE_REPRESENTATION('',(#990,#991),#33952);
#874=ADVANCED_BREP_SHAPE_REPRESENTATION('',(#992),#33953);
#875=ADVANCED_BREP_SHAPE_REPRESENTATION('',(#993),#33954);
#876=ADVANCED_BREP_SHAPE_REPRESENTATION('',(#994),#33955);
#877=ADVANCED_BREP_SHAPE_REPRESENTATION('',(#20),#33956);
#878=ADVANCED_BREP_SHAPE_REPRESENTATION('',(#995),#33958);
#879=ADVANCED_BREP_SHAPE_REPRESENTATION('',(#996),#33959);
#880=ADVANCED_BREP_SHAPE_REPRESENTATION('',(#997),#33960);
#881=ADVANCED_BREP_SHAPE_REPRESENTATION('',(#998),#33962);
#882=ADVANCED_BREP_SHAPE_REPRESENTATION('',(#999),#33963);
#883=ADVANCED_BREP_SHAPE_REPRESENTATION('',(#1000),#33964);
#884=ADVANCED_BREP_SHAPE_REPRESENTATION('',(#1001),#33965);
#885=ADVANCED_BREP_SHAPE_REPRESENTATION('',(#21),#33966);
#886=ADVANCED_BREP_SHAPE_REPRESENTATION('',(#1002),#33967);
#887=ADVANCED_BREP_SHAPE_REPRESENTATION('',(#22),#33968);
#888=ADVANCED_BREP_SHAPE_REPRESENTATION('',(#23),#33969);
#889=ADVANCED_BREP_SHAPE_REPRESENTATION('',(#1003),#33971);
#890=ADVANCED_BREP_SHAPE_REPRESENTATION('',(#1004),#33972);
#891=ADVANCED_BREP_SHAPE_REPRESENTATION('',(#1005),#33973);
#892=ADVANCED_BREP_SHAPE_REPRESENTATION('',(#1006),#33974);
#893=ADVANCED_BREP_SHAPE_REPRESENTATION('',(#1007),#33975);
#894=ADVANCED_BREP_SHAPE_REPRESENTATION('',(#1008),#33976);
#895=ADVANCED_BREP_SHAPE_REPRESENTATION('',(#1009),#33977);
#896=ADVANCED_BREP_SHAPE_REPRESENTATION('',(#1010),#33978);
#897=ADVANCED_BREP_SHAPE_REPRESENTATION('',(#1011),#33979);
#898=ADVANCED_BREP_SHAPE_REPRESENTATION('',(#24),#33980);
#899=STYLED_ITEM('',(#34496),#958);
#900=STYLED_ITEM('',(#34510),#959);
#901=STYLED_ITEM('',(#34517),#960);
#902=STYLED_ITEM('',(#34510),#961);
#903=STYLED_ITEM('',(#34517),#962);
#904=STYLED_ITEM('',(#34531),#963);
#905=STYLED_ITEM('',(#34510),#964);
#906=STYLED_ITEM('',(#34510),#965);
#907=STYLED_ITEM('',(#34510),#966);
#908=STYLED_ITEM('',(#34517),#967);
#909=STYLED_ITEM('',(#34517),#968);
#910=STYLED_ITEM('',(#34517),#969);
#911=STYLED_ITEM('',(#34517),#970);
#912=STYLED_ITEM('',(#34517),#971);
#913=STYLED_ITEM('',(#34517),#972);
#914=STYLED_ITEM('',(#34517),#973);
#915=STYLED_ITEM('',(#34517),#974);
#916=STYLED_ITEM('',(#34517),#975);
#917=STYLED_ITEM('',(#34517),#976);
#918=STYLED_ITEM('',(#34517),#977);
#919=STYLED_ITEM('',(#34517),#978);
#920=STYLED_ITEM('',(#34517),#979);
#921=STYLED_ITEM('',(#34517),#980);
#922=STYLED_ITEM('',(#34517),#981);
#923=STYLED_ITEM('',(#34517),#982);
#924=STYLED_ITEM('',(#34517),#983);
#925=STYLED_ITEM('',(#34517),#984);
#926=STYLED_ITEM('',(#34517),#985);
#927=STYLED_ITEM('',(#34517),#986);
#928=STYLED_ITEM('',(#34517),#987);
#929=STYLED_ITEM('',(#34517),#988);
#930=STYLED_ITEM('',(#34517),#989);
#931=STYLED_ITEM('',(#34517),#990);
#932=STYLED_ITEM('',(#34517),#991);
#933=STYLED_ITEM('',(#34531),#992);
#934=STYLED_ITEM('',(#34524),#993);
#935=STYLED_ITEM('',(#34524),#994);
#936=STYLED_ITEM('',(#34524),#20);
#937=STYLED_ITEM('',(#34510),#995);
#938=STYLED_ITEM('',(#34531),#996);
#939=STYLED_ITEM('',(#34524),#997);
#940=STYLED_ITEM('',(#34496),#998);
#941=STYLED_ITEM('',(#34510),#999);
#942=STYLED_ITEM('',(#34531),#1000);
#943=STYLED_ITEM('',(#34524),#1001);
#944=STYLED_ITEM('',(#34524),#21);
#945=STYLED_ITEM('',(#34524),#1002);
#946=STYLED_ITEM('',(#34524),#22);
#947=STYLED_ITEM('',(#34524),#23);
#948=STYLED_ITEM('',(#34524),#1003);
#949=STYLED_ITEM('',(#34517),#1004);
#950=STYLED_ITEM('',(#34517),#1005);
#951=STYLED_ITEM('',(#34510),#1006);
#952=STYLED_ITEM('',(#34510),#1007);
#953=STYLED_ITEM('',(#34510),#1008);
#954=STYLED_ITEM('',(#34517),#1009);
#955=STYLED_ITEM('',(#34524),#1010);
#956=STYLED_ITEM('',(#34524),#1011);
#957=STYLED_ITEM('',(#34524),#24);
#958=MANIFOLD_SOLID_BREP('Body1',#13010);
#959=MANIFOLD_SOLID_BREP('Body1',#13011);
#960=MANIFOLD_SOLID_BREP('Body1',#13012);
#961=MANIFOLD_SOLID_BREP('Body1',#13013);
#962=MANIFOLD_SOLID_BREP('Body1',#13014);
#963=MANIFOLD_SOLID_BREP('Body1',#13015);
#964=MANIFOLD_SOLID_BREP('Body1',#13016);
#965=MANIFOLD_SOLID_BREP('Body1',#13017);
#966=MANIFOLD_SOLID_BREP('Body1',#13018);
#967=MANIFOLD_SOLID_BREP('Body1',#13019);
#968=MANIFOLD_SOLID_BREP('Body1',#13020);
#969=MANIFOLD_SOLID_BREP('Body1',#13021);
#970=MANIFOLD_SOLID_BREP('Body2',#13022);
#971=MANIFOLD_SOLID_BREP('Body3',#13023);
#972=MANIFOLD_SOLID_BREP('Body4',#13024);
#973=MANIFOLD_SOLID_BREP('Body5',#13025);
#974=MANIFOLD_SOLID_BREP('Body6',#13026);
#975=MANIFOLD_SOLID_BREP('Body7',#13027);
#976=MANIFOLD_SOLID_BREP('Continuous crown cage',#13028);
#977=MANIFOLD_SOLID_BREP('Body1',#13029);
#978=MANIFOLD_SOLID_BREP('Body2',#13030);
#979=MANIFOLD_SOLID_BREP('Body1',#13031);
#980=MANIFOLD_SOLID_BREP('Body1',#13032);
#981=MANIFOLD_SOLID_BREP('Body1',#13033);
#982=MANIFOLD_SOLID_BREP('Body2',#13034);
#983=MANIFOLD_SOLID_BREP('Body3',#13035);
#984=MANIFOLD_SOLID_BREP('Body4',#13036);
#985=MANIFOLD_SOLID_BREP('Body5',#13037);
#986=MANIFOLD_SOLID_BREP('Body6',#13038);
#987=MANIFOLD_SOLID_BREP('Body7',#13039);
#988=MANIFOLD_SOLID_BREP('Body8',#13040);
#989=MANIFOLD_SOLID_BREP('Continuous crown cage',#13041);
#990=MANIFOLD_SOLID_BREP('Body1',#13042);
#991=MANIFOLD_SOLID_BREP('Body2',#13043);
#992=MANIFOLD_SOLID_BREP('Body1',#13044);
#993=MANIFOLD_SOLID_BREP('Body1',#13045);
#994=MANIFOLD_SOLID_BREP('Body1',#13046);
#995=MANIFOLD_SOLID_BREP('Body1',#13049);
#996=MANIFOLD_SOLID_BREP('Body1',#13050);
#997=MANIFOLD_SOLID_BREP('Body1',#13051);
#998=MANIFOLD_SOLID_BREP('Body1',#13052);
#999=MANIFOLD_SOLID_BREP('Body1',#13053);
#1000=MANIFOLD_SOLID_BREP('Body1',#13054);
#1001=MANIFOLD_SOLID_BREP('Body1',#13055);
#1002=MANIFOLD_SOLID_BREP('Body1',#13058);
#1003=MANIFOLD_SOLID_BREP('Body1',#13063);
#1004=MANIFOLD_SOLID_BREP('Body1',#13064);
#1005=MANIFOLD_SOLID_BREP('Body1',#13065);
#1006=MANIFOLD_SOLID_BREP('Body1',#13066);
#1007=MANIFOLD_SOLID_BREP('Body1',#13067);
#1008=MANIFOLD_SOLID_BREP('Body1',#13068);
#1009=MANIFOLD_SOLID_BREP('Body1',#13069);
#1010=MANIFOLD_SOLID_BREP('Body1',#13070);
#1011=MANIFOLD_SOLID_BREP('Body1',#13071);
#1012=FACE_BOUND('',#2319,.T.);
#1013=FACE_BOUND('',#2320,.T.);
#1014=FACE_BOUND('',#2321,.T.);
#1015=FACE_BOUND('',#2322,.T.);
#1016=FACE_BOUND('',#2323,.T.);
#1017=FACE_BOUND('',#2324,.T.);
#1018=FACE_BOUND('',#2325,.T.);
#1019=FACE_BOUND('',#2326,.T.);
#1020=FACE_BOUND('',#2327,.T.);
#1021=FACE_BOUND('',#2328,.T.);
#1022=FACE_BOUND('',#2329,.T.);
#1023=FACE_BOUND('',#2330,.T.);
#1024=FACE_BOUND('',#2331,.T.);
#1025=FACE_BOUND('',#2332,.T.);
#1026=FACE_BOUND('',#2333,.T.);
#1027=FACE_BOUND('',#2334,.T.);
#1028=FACE_BOUND('',#2336,.T.);
#1029=FACE_BOUND('',#2337,.T.);
#1030=FACE_BOUND('',#2338,.T.);
#1031=FACE_BOUND('',#2339,.T.);
#1032=FACE_BOUND('',#2340,.T.);
#1033=FACE_BOUND('',#2341,.T.);
#1034=FACE_BOUND('',#2342,.T.);
#1035=FACE_BOUND('',#2343,.T.);
#1036=FACE_BOUND('',#2344,.T.);
#1037=FACE_BOUND('',#2345,.T.);
#1038=FACE_BOUND('',#2346,.T.);
#1039=FACE_BOUND('',#2347,.T.);
#1040=FACE_BOUND('',#2348,.T.);
#1041=FACE_BOUND('',#2349,.T.);
#1042=FACE_BOUND('',#2350,.T.);
#1043=FACE_BOUND('',#2351,.T.);
#1044=FACE_BOUND('',#2358,.T.);
#1045=FACE_BOUND('',#2361,.T.);
#1046=FACE_BOUND('',#2364,.T.);
#1047=FACE_BOUND('',#2367,.T.);
#1048=FACE_BOUND('',#2377,.T.);
#1049=FACE_BOUND('',#2378,.T.);
#1050=FACE_BOUND('',#2379,.T.);
#1051=FACE_BOUND('',#2380,.T.);
#1052=FACE_BOUND('',#2381,.T.);
#1053=FACE_BOUND('',#2382,.T.);
#1054=FACE_BOUND('',#2383,.T.);
#1055=FACE_BOUND('',#2384,.T.);
#1056=FACE_BOUND('',#2386,.T.);
#1057=FACE_BOUND('',#2387,.T.);
#1058=FACE_BOUND('',#2388,.T.);
#1059=FACE_BOUND('',#2389,.T.);
#1060=FACE_BOUND('',#2390,.T.);
#1061=FACE_BOUND('',#2391,.T.);
#1062=FACE_BOUND('',#2392,.T.);
#1063=FACE_BOUND('',#2393,.T.);
#1064=FACE_BOUND('',#2399,.T.);
#1065=FACE_BOUND('',#2407,.T.);
#1066=FACE_BOUND('',#2408,.T.);
#1067=FACE_BOUND('',#2409,.T.);
#1068=FACE_BOUND('',#2410,.T.);
#1069=FACE_BOUND('',#2413,.T.);
#1070=FACE_BOUND('',#2414,.T.);
#1071=FACE_BOUND('',#2415,.T.);
#1072=FACE_BOUND('',#2416,.T.);
#1073=FACE_BOUND('',#2419,.T.);
#1074=FACE_BOUND('',#2420,.T.);
#1075=FACE_BOUND('',#2426,.T.);
#1076=FACE_BOUND('',#2430,.T.);
#1077=FACE_BOUND('',#2431,.T.);
#1078=FACE_BOUND('',#2432,.T.);
#1079=FACE_BOUND('',#2433,.T.);
#1080=FACE_BOUND('',#2435,.T.);
#1081=FACE_BOUND('',#2436,.T.);
#1082=FACE_BOUND('',#2437,.T.);
#1083=FACE_BOUND('',#2438,.T.);
#1084=FACE_BOUND('',#2444,.T.);
#1085=FACE_BOUND('',#2452,.T.);
#1086=FACE_BOUND('',#2453,.T.);
#1087=FACE_BOUND('',#2454,.T.);
#1088=FACE_BOUND('',#2455,.T.);
#1089=FACE_BOUND('',#2458,.T.);
#1090=FACE_BOUND('',#2459,.T.);
#1091=FACE_BOUND('',#2460,.T.);
#1092=FACE_BOUND('',#2461,.T.);
#1093=FACE_BOUND('',#2464,.T.);
#1094=FACE_BOUND('',#2465,.T.);
#1095=FACE_BOUND('',#2468,.T.);
#1096=FACE_BOUND('',#2469,.T.);
#1097=FACE_BOUND('',#2470,.T.);
#1098=FACE_BOUND('',#2471,.T.);
#1099=FACE_BOUND('',#2478,.T.);
#1100=FACE_BOUND('',#2481,.T.);
#1101=FACE_BOUND('',#2482,.T.);
#1102=FACE_BOUND('',#2483,.T.);
#1103=FACE_BOUND('',#2484,.T.);
#1104=FACE_BOUND('',#2486,.T.);
#1105=FACE_BOUND('',#2489,.T.);
#1106=FACE_BOUND('',#2498,.T.);
#1107=FACE_BOUND('',#2503,.T.);
#1108=FACE_BOUND('',#2504,.T.);
#1109=FACE_BOUND('',#2506,.T.);
#1110=FACE_BOUND('',#2508,.T.);
#1111=FACE_BOUND('',#2511,.T.);
#1112=FACE_BOUND('',#2520,.T.);
#1113=FACE_BOUND('',#2525,.T.);
#1114=FACE_BOUND('',#2526,.T.);
#1115=FACE_BOUND('',#2528,.T.);
#1116=FACE_BOUND('',#2531,.T.);
#1117=FACE_BOUND('',#2534,.T.);
#1118=FACE_BOUND('',#2537,.T.);
#1119=FACE_BOUND('',#2540,.T.);
#1120=FACE_BOUND('',#2550,.T.);
#1121=FACE_BOUND('',#2551,.T.);
#1122=FACE_BOUND('',#2552,.T.);
#1123=FACE_BOUND('',#2553,.T.);
#1124=FACE_BOUND('',#2560,.T.);
#1125=FACE_BOUND('',#2561,.T.);
#1126=FACE_BOUND('',#2562,.T.);
#1127=FACE_BOUND('',#2563,.T.);
#1128=FACE_BOUND('',#2572,.T.);
#1129=FACE_BOUND('',#2575,.T.);
#1130=FACE_BOUND('',#2580,.T.);
#1131=FACE_BOUND('',#2585,.T.);
#1132=FACE_BOUND('',#2610,.T.);
#1133=FACE_BOUND('',#2613,.T.);
#1134=FACE_BOUND('',#2616,.T.);
#1135=FACE_BOUND('',#2619,.T.);
#1136=FACE_BOUND('',#2622,.T.);
#1137=FACE_BOUND('',#2629,.T.);
#1138=FACE_BOUND('',#2632,.T.);
#1139=FACE_BOUND('',#2637,.T.);
#1140=FACE_BOUND('',#2642,.T.);
#1141=FACE_BOUND('',#2670,.T.);
#1142=FACE_BOUND('',#2673,.T.);
#1143=FACE_BOUND('',#2676,.T.);
#1144=FACE_BOUND('',#2679,.T.);
#1145=FACE_BOUND('',#2682,.T.);
#1146=FACE_BOUND('',#2730,.T.);
#1147=FACE_BOUND('',#2732,.T.);
#1148=FACE_BOUND('',#2743,.T.);
#1149=FACE_BOUND('',#2747,.T.);
#1150=FACE_BOUND('',#2750,.T.);
#1151=FACE_BOUND('',#2765,.T.);
#1152=FACE_BOUND('',#2777,.T.);
#1153=FACE_BOUND('',#2778,.T.);
#1154=FACE_BOUND('',#2779,.T.);
#1155=FACE_BOUND('',#2780,.T.);
#1156=FACE_BOUND('',#2782,.T.);
#1157=FACE_BOUND('',#2783,.T.);
#1158=FACE_BOUND('',#2784,.T.);
#1159=FACE_BOUND('',#2785,.T.);
#1160=FACE_BOUND('',#2799,.T.);
#1161=FACE_BOUND('',#2800,.T.);
#1162=FACE_BOUND('',#2801,.T.);
#1163=FACE_BOUND('',#2802,.T.);
#1164=FACE_BOUND('',#2803,.T.);
#1165=FACE_BOUND('',#2804,.T.);
#1166=FACE_BOUND('',#2805,.T.);
#1167=FACE_BOUND('',#2806,.T.);
#1168=FACE_BOUND('',#2808,.T.);
#1169=FACE_BOUND('',#2809,.T.);
#1170=FACE_BOUND('',#2810,.T.);
#1171=FACE_BOUND('',#2811,.T.);
#1172=FACE_BOUND('',#2812,.T.);
#1173=FACE_BOUND('',#2813,.T.);
#1174=FACE_BOUND('',#2814,.T.);
#1175=FACE_BOUND('',#2815,.T.);
#1176=FACE_BOUND('',#2833,.T.);
#1177=FACE_BOUND('',#2834,.T.);
#1178=FACE_BOUND('',#2835,.T.);
#1179=FACE_BOUND('',#2836,.T.);
#1180=FACE_BOUND('',#2839,.T.);
#1181=FACE_BOUND('',#2841,.T.);
#1182=FACE_BOUND('',#2842,.T.);
#1183=FACE_BOUND('',#2843,.T.);
#1184=FACE_BOUND('',#2844,.T.);
#1185=FACE_BOUND('',#2860,.T.);
#1186=FACE_BOUND('',#2861,.T.);
#1187=FACE_BOUND('',#2862,.T.);
#1188=FACE_BOUND('',#2863,.T.);
#1189=FACE_BOUND('',#2895,.T.);
#1190=FACE_BOUND('',#2898,.T.);
#1191=FACE_BOUND('',#2908,.T.);
#1192=FACE_BOUND('',#2916,.T.);
#1193=FACE_BOUND('',#2941,.T.);
#1194=FACE_BOUND('',#2942,.T.);
#1195=FACE_BOUND('',#2943,.T.);
#1196=FACE_BOUND('',#2944,.T.);
#1197=FACE_BOUND('',#2950,.T.);
#1198=FACE_BOUND('',#2951,.T.);
#1199=FACE_BOUND('',#2952,.T.);
#1200=FACE_BOUND('',#2953,.T.);
#1201=FACE_BOUND('',#2958,.T.);
#1202=FACE_BOUND('',#2964,.T.);
#1203=FACE_BOUND('',#2982,.T.);
#1204=FACE_BOUND('',#3122,.T.);
#1205=FACE_BOUND('',#3134,.T.);
#1206=FACE_BOUND('',#3137,.T.);
#1207=FACE_BOUND('',#3140,.T.);
#1208=FACE_BOUND('',#3145,.T.);
#1209=FACE_BOUND('',#3147,.T.);
#1210=FACE_BOUND('',#3152,.T.);
#1211=FACE_BOUND('',#3154,.T.);
#1212=FACE_BOUND('',#3156,.T.);
#1213=FACE_BOUND('',#3158,.T.);
#1214=FACE_BOUND('',#3167,.T.);
#1215=FACE_BOUND('',#3168,.T.);
#1216=FACE_BOUND('',#3170,.T.);
#1217=FACE_BOUND('',#3171,.T.);
#1218=FACE_BOUND('',#3174,.T.);
#1219=FACE_BOUND('',#3176,.T.);
#1220=FACE_BOUND('',#3181,.T.);
#1221=FACE_BOUND('',#3183,.T.);
#1222=FACE_BOUND('',#3187,.T.);
#1223=FACE_BOUND('',#3189,.T.);
#1224=FACE_BOUND('',#3208,.T.);
#1225=FACE_BOUND('',#3216,.T.);
#1226=FACE_BOUND('',#3218,.T.);
#1227=FACE_BOUND('',#3224,.T.);
#1228=PLANE('',#13610);
#1229=PLANE('',#13611);
#1230=PLANE('',#13612);
#1231=PLANE('',#13613);
#1232=PLANE('',#13614);
#1233=PLANE('',#13615);
#1234=PLANE('',#13632);
#1235=PLANE('',#13637);
#1236=PLANE('',#13642);
#1237=PLANE('',#13647);
#1238=PLANE('',#13657);
#1239=PLANE('',#13658);
#1240=PLANE('',#13659);
#1241=PLANE('',#13660);
#1242=PLANE('',#13661);
#1243=PLANE('',#13662);
#1244=PLANE('',#13676);
#1245=PLANE('',#13683);
#1246=PLANE('',#13687);
#1247=PLANE('',#13688);
#1248=PLANE('',#13689);
#1249=PLANE('',#13690);
#1250=PLANE('',#13691);
#1251=PLANE('',#13692);
#1252=PLANE('',#13693);
#1253=PLANE('',#13707);
#1254=PLANE('',#13714);
#1255=PLANE('',#13715);
#1256=PLANE('',#13729);
#1257=PLANE('',#13736);
#1258=PLANE('',#13740);
#1259=PLANE('',#13741);
#1260=PLANE('',#13742);
#1261=PLANE('',#13743);
#1262=PLANE('',#13744);
#1263=PLANE('',#13745);
#1264=PLANE('',#13746);
#1265=PLANE('',#13748);
#1266=PLANE('',#13749);
#1267=PLANE('',#13765);
#1268=PLANE('',#13769);
#1269=PLANE('',#13771);
#1270=PLANE('',#13778);
#1271=PLANE('',#13785);
#1272=PLANE('',#13786);
#1273=PLANE('',#13791);
#1274=PLANE('',#13792);
#1275=PLANE('',#13793);
#1276=PLANE('',#13794);
#1277=PLANE('',#13795);
#1278=PLANE('',#13796);
#1279=PLANE('',#13797);
#1280=PLANE('',#13798);
#1281=PLANE('',#13800);
#1282=PLANE('',#13807);
#1283=PLANE('',#13814);
#1284=PLANE('',#13815);
#1285=PLANE('',#13820);
#1286=PLANE('',#13821);
#1287=PLANE('',#13822);
#1288=PLANE('',#13823);
#1289=PLANE('',#13824);
#1290=PLANE('',#13825);
#1291=PLANE('',#13826);
#1292=PLANE('',#13827);
#1293=PLANE('',#13832);
#1294=PLANE('',#13837);
#1295=PLANE('',#13842);
#1296=PLANE('',#13847);
#1297=PLANE('',#13857);
#1298=PLANE('',#13858);
#1299=PLANE('',#13859);
#1300=PLANE('',#13860);
#1301=PLANE('',#13861);
#1302=PLANE('',#13862);
#1303=PLANE('',#13863);
#1304=PLANE('',#13864);
#1305=PLANE('',#13865);
#1306=PLANE('',#13866);
#1307=PLANE('',#13867);
#1308=PLANE('',#13868);
#1309=PLANE('',#13869);
#1310=PLANE('',#13870);
#1311=PLANE('',#13886);
#1312=PLANE('',#13889);
#1313=PLANE('',#13901);
#1314=PLANE('',#13910);
#1315=PLANE('',#13941);
#1316=PLANE('',#13946);
#1317=PLANE('',#13951);
#1318=PLANE('',#13957);
#1319=PLANE('',#13962);
#1320=PLANE('',#13971);
#1321=PLANE('',#13975);
#1322=PLANE('',#13976);
#1323=PLANE('',#13978);
#1324=PLANE('',#13983);
#1325=PLANE('',#13986);
#1326=PLANE('',#13991);
#1327=PLANE('',#14014);
#1328=PLANE('',#14017);
#1329=PLANE('',#14029);
#1330=PLANE('',#14038);
#1331=PLANE('',#14071);
#1332=PLANE('',#14076);
#1333=PLANE('',#14081);
#1334=PLANE('',#14086);
#1335=PLANE('',#14091);
#1336=PLANE('',#14096);
#1337=PLANE('',#14105);
#1338=PLANE('',#14109);
#1339=PLANE('',#14110);
#1340=PLANE('',#14112);
#1341=PLANE('',#14117);
#1342=PLANE('',#14120);
#1343=PLANE('',#14125);
#1344=PLANE('',#14134);
#1345=PLANE('',#14135);
#1346=PLANE('',#14136);
#1347=PLANE('',#14137);
#1348=PLANE('',#14138);
#1349=PLANE('',#14139);
#1350=PLANE('',#14140);
#1351=PLANE('',#14141);
#1352=PLANE('',#14142);
#1353=PLANE('',#14143);
#1354=PLANE('',#14144);
#1355=PLANE('',#14145);
#1356=PLANE('',#14146);
#1357=PLANE('',#14147);
#1358=PLANE('',#14148);
#1359=PLANE('',#14149);
#1360=PLANE('',#14150);
#1361=PLANE('',#14151);
#1362=PLANE('',#14152);
#1363=PLANE('',#14153);
#1364=PLANE('',#14154);
#1365=PLANE('',#14155);
#1366=PLANE('',#14156);
#1367=PLANE('',#14157);
#1368=PLANE('',#14158);
#1369=PLANE('',#14159);
#1370=PLANE('',#14160);
#1371=PLANE('',#14161);
#1372=PLANE('',#14162);
#1373=PLANE('',#14163);
#1374=PLANE('',#14164);
#1375=PLANE('',#14165);
#1376=PLANE('',#14166);
#1377=PLANE('',#14167);
#1378=PLANE('',#14168);
#1379=PLANE('',#14169);
#1380=PLANE('',#14173);
#1381=PLANE('',#14174);
#1382=PLANE('',#14175);
#1383=PLANE('',#14176);
#1384=PLANE('',#14177);
#1385=PLANE('',#14178);
#1386=PLANE('',#14179);
#1387=PLANE('',#14180);
#1388=PLANE('',#14181);
#1389=PLANE('',#14182);
#1390=PLANE('',#14184);
#1391=PLANE('',#14192);
#1392=PLANE('',#14193);
#1393=PLANE('',#14194);
#1394=PLANE('',#14195);
#1395=PLANE('',#14196);
#1396=PLANE('',#14197);
#1397=PLANE('',#14198);
#1398=PLANE('',#14199);
#1399=PLANE('',#14206);
#1400=PLANE('',#14210);
#1401=PLANE('',#14212);
#1402=PLANE('',#14213);
#1403=PLANE('',#14214);
#1404=PLANE('',#14215);
#1405=PLANE('',#14216);
#1406=PLANE('',#14217);
#1407=PLANE('',#14218);
#1408=PLANE('',#14219);
#1409=PLANE('',#14220);
#1410=PLANE('',#14222);
#1411=PLANE('',#14230);
#1412=PLANE('',#14249);
#1413=PLANE('',#14250);
#1414=PLANE('',#14251);
#1415=PLANE('',#14252);
#1416=PLANE('',#14253);
#1417=PLANE('',#14254);
#1418=PLANE('',#14280);
#1419=PLANE('',#14281);
#1420=PLANE('',#14282);
#1421=PLANE('',#14283);
#1422=PLANE('',#14284);
#1423=PLANE('',#14285);
#1424=PLANE('',#14290);
#1425=PLANE('',#14294);
#1426=PLANE('',#14298);
#1427=PLANE('',#14302);
#1428=PLANE('',#14306);
#1429=PLANE('',#14310);
#1430=PLANE('',#14314);
#1431=PLANE('',#14318);
#1432=PLANE('',#14319);
#1433=PLANE('',#14320);
#1434=PLANE('',#14321);
#1435=PLANE('',#14322);
#1436=PLANE('',#14323);
#1437=PLANE('',#14326);
#1438=PLANE('',#14332);
#1439=PLANE('',#14338);
#1440=PLANE('',#14344);
#1441=PLANE('',#14350);
#1442=PLANE('',#14351);
#1443=PLANE('',#14352);
#1444=PLANE('',#14353);
#1445=PLANE('',#14354);
#1446=PLANE('',#14355);
#1447=PLANE('',#14356);
#1448=PLANE('',#14357);
#1449=PLANE('',#14358);
#1450=PLANE('',#14359);
#1451=PLANE('',#14360);
#1452=PLANE('',#14361);
#1453=PLANE('',#14362);
#1454=PLANE('',#14363);
#1455=PLANE('',#14365);
#1456=PLANE('',#14366);
#1457=PLANE('',#14367);
#1458=PLANE('',#14368);
#1459=PLANE('',#14369);
#1460=PLANE('',#14370);
#1461=PLANE('',#14371);
#1462=PLANE('',#14372);
#1463=PLANE('',#14373);
#1464=PLANE('',#14374);
#1465=PLANE('',#14376);
#1466=PLANE('',#14377);
#1467=PLANE('',#14378);
#1468=PLANE('',#14379);
#1469=PLANE('',#14380);
#1470=PLANE('',#14381);
#1471=PLANE('',#14382);
#1472=PLANE('',#14383);
#1473=PLANE('',#14384);
#1474=PLANE('',#14385);
#1475=PLANE('',#14395);
#1476=PLANE('',#14399);
#1477=PLANE('',#14401);
#1478=PLANE('',#14402);
#1479=PLANE('',#14403);
#1480=PLANE('',#14404);
#1481=PLANE('',#14405);
#1482=PLANE('',#14406);
#1483=PLANE('',#14407);
#1484=PLANE('',#14408);
#1485=PLANE('',#14409);
#1486=PLANE('',#14414);
#1487=PLANE('',#14415);
#1488=PLANE('',#14423);
#1489=PLANE('',#14452);
#1490=PLANE('',#14464);
#1491=PLANE('',#14465);
#1492=PLANE('',#14472);
#1493=PLANE('',#14474);
#1494=PLANE('',#14482);
#1495=PLANE('',#14490);
#1496=PLANE('',#14491);
#1497=PLANE('',#14492);
#1498=PLANE('',#14493);
#1499=PLANE('',#14494);
#1500=PLANE('',#14495);
#1501=PLANE('',#14496);
#1502=PLANE('',#14497);
#1503=PLANE('',#14498);
#1504=PLANE('',#14500);
#1505=PLANE('',#14508);
#1506=PLANE('',#14516);
#1507=PLANE('',#14517);
#1508=PLANE('',#14518);
#1509=PLANE('',#14519);
#1510=PLANE('',#14520);
#1511=PLANE('',#14521);
#1512=PLANE('',#14522);
#1513=PLANE('',#14523);
#1514=PLANE('',#14524);
#1515=PLANE('',#14676);
#1516=PLANE('',#14681);
#1517=PLANE('',#14683);
#1518=PLANE('',#14684);
#1519=PLANE('',#14686);
#1520=PLANE('',#14687);
#1521=PLANE('',#14688);
#1522=PLANE('',#14693);
#1523=PLANE('',#14694);
#1524=PLANE('',#14699);
#1525=PLANE('',#14708);
#1526=PLANE('',#14709);
#1527=PLANE('',#14711);
#1528=PLANE('',#14715);
#1529=PLANE('',#14722);
#1530=PLANE('',#14723);
#1531=PLANE('',#14728);
#1532=PLANE('',#14732);
#1533=PLANE('',#14733);
#1534=PLANE('',#14734);
#1535=PLANE('',#14735);
#1536=PLANE('',#14736);
#1537=PLANE('',#14739);
#1538=PLANE('',#14747);
#1539=PLANE('',#14755);
#1540=PLANE('',#14756);
#1541=PLANE('',#14764);
#1542=PLANE('',#14765);
#1543=PLANE('',#14767);
#1544=PLANE('',#14768);
#1545=PLANE('',#14769);
#1546=PLANE('',#14770);
#1547=PLANE('',#14771);
#1548=PLANE('',#14772);
#1549=PLANE('',#14773);
#1550=PLANE('',#14774);
#1551=PLANE('',#14775);
#1552=PLANE('',#14776);
#1553=PLANE('',#14778);
#1554=PLANE('',#14779);
#1555=PLANE('',#14780);
#1556=PLANE('',#14781);
#1557=PLANE('',#14782);
#1558=PLANE('',#14783);
#1559=PLANE('',#14784);
#1560=PLANE('',#14785);
#1561=PLANE('',#14793);
#1562=PLANE('',#14801);
#1563=PLANE('',#14802);
#1564=PLANE('',#14804);
#1565=PLANE('',#14812);
#1566=PLANE('',#14820);
#1567=PLANE('',#14821);
#1568=PLANE('',#14822);
#1569=PLANE('',#14823);
#1570=PLANE('',#14824);
#1571=PLANE('',#14825);
#1572=PLANE('',#14826);
#1573=PLANE('',#14827);
#1574=PLANE('',#14828);
#1575=FACE_OUTER_BOUND('',#2298,.T.);
#1576=FACE_OUTER_BOUND('',#2299,.T.);
#1577=FACE_OUTER_BOUND('',#2300,.T.);
#1578=FACE_OUTER_BOUND('',#2301,.T.);
#1579=FACE_OUTER_BOUND('',#2302,.T.);
#1580=FACE_OUTER_BOUND('',#2303,.T.);
#1581=FACE_OUTER_BOUND('',#2304,.T.);
#1582=FACE_OUTER_BOUND('',#2305,.T.);
#1583=FACE_OUTER_BOUND('',#2306,.T.);
#1584=FACE_OUTER_BOUND('',#2307,.T.);
#1585=FACE_OUTER_BOUND('',#2308,.T.);
#1586=FACE_OUTER_BOUND('',#2309,.T.);
#1587=FACE_OUTER_BOUND('',#2310,.T.);
#1588=FACE_OUTER_BOUND('',#2311,.T.);
#1589=FACE_OUTER_BOUND('',#2312,.T.);
#1590=FACE_OUTER_BOUND('',#2313,.T.);
#1591=FACE_OUTER_BOUND('',#2314,.T.);
#1592=FACE_OUTER_BOUND('',#2315,.T.);
#1593=FACE_OUTER_BOUND('',#2316,.T.);
#1594=FACE_OUTER_BOUND('',#2317,.T.);
#1595=FACE_OUTER_BOUND('',#2318,.T.);
#1596=FACE_OUTER_BOUND('',#2335,.T.);
#1597=FACE_OUTER_BOUND('',#2352,.T.);
#1598=FACE_OUTER_BOUND('',#2353,.T.);
#1599=FACE_OUTER_BOUND('',#2354,.T.);
#1600=FACE_OUTER_BOUND('',#2355,.T.);
#1601=FACE_OUTER_BOUND('',#2356,.T.);
#1602=FACE_OUTER_BOUND('',#2357,.T.);
#1603=FACE_OUTER_BOUND('',#2359,.T.);
#1604=FACE_OUTER_BOUND('',#2360,.T.);
#1605=FACE_OUTER_BOUND('',#2362,.T.);
#1606=FACE_OUTER_BOUND('',#2363,.T.);
#1607=FACE_OUTER_BOUND('',#2365,.T.);
#1608=FACE_OUTER_BOUND('',#2366,.T.);
#1609=FACE_OUTER_BOUND('',#2368,.T.);
#1610=FACE_OUTER_BOUND('',#2369,.T.);
#1611=FACE_OUTER_BOUND('',#2370,.T.);
#1612=FACE_OUTER_BOUND('',#2371,.T.);
#1613=FACE_OUTER_BOUND('',#2372,.T.);
#1614=FACE_OUTER_BOUND('',#2373,.T.);
#1615=FACE_OUTER_BOUND('',#2374,.T.);
#1616=FACE_OUTER_BOUND('',#2375,.T.);
#1617=FACE_OUTER_BOUND('',#2376,.T.);
#1618=FACE_OUTER_BOUND('',#2385,.T.);
#1619=FACE_OUTER_BOUND('',#2394,.T.);
#1620=FACE_OUTER_BOUND('',#2395,.T.);
#1621=FACE_OUTER_BOUND('',#2396,.T.);
#1622=FACE_OUTER_BOUND('',#2397,.T.);
#1623=FACE_OUTER_BOUND('',#2398,.T.);
#1624=FACE_OUTER_BOUND('',#2400,.T.);
#1625=FACE_OUTER_BOUND('',#2401,.T.);
#1626=FACE_OUTER_BOUND('',#2402,.T.);
#1627=FACE_OUTER_BOUND('',#2403,.T.);
#1628=FACE_OUTER_BOUND('',#2404,.T.);
#1629=FACE_OUTER_BOUND('',#2405,.T.);
#1630=FACE_OUTER_BOUND('',#2406,.T.);
#1631=FACE_OUTER_BOUND('',#2411,.T.);
#1632=FACE_OUTER_BOUND('',#2412,.T.);
#1633=FACE_OUTER_BOUND('',#2417,.T.);
#1634=FACE_OUTER_BOUND('',#2418,.T.);
#1635=FACE_OUTER_BOUND('',#2421,.T.);
#1636=FACE_OUTER_BOUND('',#2422,.T.);
#1637=FACE_OUTER_BOUND('',#2423,.T.);
#1638=FACE_OUTER_BOUND('',#2424,.T.);
#1639=FACE_OUTER_BOUND('',#2425,.T.);
#1640=FACE_OUTER_BOUND('',#2427,.T.);
#1641=FACE_OUTER_BOUND('',#2428,.T.);
#1642=FACE_OUTER_BOUND('',#2429,.T.);
#1643=FACE_OUTER_BOUND('',#2434,.T.);
#1644=FACE_OUTER_BOUND('',#2439,.T.);
#1645=FACE_OUTER_BOUND('',#2440,.T.);
#1646=FACE_OUTER_BOUND('',#2441,.T.);
#1647=FACE_OUTER_BOUND('',#2442,.T.);
#1648=FACE_OUTER_BOUND('',#2443,.T.);
#1649=FACE_OUTER_BOUND('',#2445,.T.);
#1650=FACE_OUTER_BOUND('',#2446,.T.);
#1651=FACE_OUTER_BOUND('',#2447,.T.);
#1652=FACE_OUTER_BOUND('',#2448,.T.);
#1653=FACE_OUTER_BOUND('',#2449,.T.);
#1654=FACE_OUTER_BOUND('',#2450,.T.);
#1655=FACE_OUTER_BOUND('',#2451,.T.);
#1656=FACE_OUTER_BOUND('',#2456,.T.);
#1657=FACE_OUTER_BOUND('',#2457,.T.);
#1658=FACE_OUTER_BOUND('',#2462,.T.);
#1659=FACE_OUTER_BOUND('',#2463,.T.);
#1660=FACE_OUTER_BOUND('',#2466,.T.);
#1661=FACE_OUTER_BOUND('',#2467,.T.);
#1662=FACE_OUTER_BOUND('',#2472,.T.);
#1663=FACE_OUTER_BOUND('',#2473,.T.);
#1664=FACE_OUTER_BOUND('',#2474,.T.);
#1665=FACE_OUTER_BOUND('',#2475,.T.);
#1666=FACE_OUTER_BOUND('',#2476,.T.);
#1667=FACE_OUTER_BOUND('',#2477,.T.);
#1668=FACE_OUTER_BOUND('',#2479,.T.);
#1669=FACE_OUTER_BOUND('',#2480,.T.);
#1670=FACE_OUTER_BOUND('',#2485,.T.);
#1671=FACE_OUTER_BOUND('',#2487,.T.);
#1672=FACE_OUTER_BOUND('',#2488,.T.);
#1673=FACE_OUTER_BOUND('',#2490,.T.);
#1674=FACE_OUTER_BOUND('',#2491,.T.);
#1675=FACE_OUTER_BOUND('',#2492,.T.);
#1676=FACE_OUTER_BOUND('',#2493,.T.);
#1677=FACE_OUTER_BOUND('',#2494,.T.);
#1678=FACE_OUTER_BOUND('',#2495,.T.);
#1679=FACE_OUTER_BOUND('',#2496,.T.);
#1680=FACE_OUTER_BOUND('',#2497,.T.);
#1681=FACE_OUTER_BOUND('',#2499,.T.);
#1682=FACE_OUTER_BOUND('',#2500,.T.);
#1683=FACE_OUTER_BOUND('',#2501,.T.);
#1684=FACE_OUTER_BOUND('',#2502,.T.);
#1685=FACE_OUTER_BOUND('',#2505,.T.);
#1686=FACE_OUTER_BOUND('',#2507,.T.);
#1687=FACE_OUTER_BOUND('',#2509,.T.);
#1688=FACE_OUTER_BOUND('',#2510,.T.);
#1689=FACE_OUTER_BOUND('',#2512,.T.);
#1690=FACE_OUTER_BOUND('',#2513,.T.);
#1691=FACE_OUTER_BOUND('',#2514,.T.);
#1692=FACE_OUTER_BOUND('',#2515,.T.);
#1693=FACE_OUTER_BOUND('',#2516,.T.);
#1694=FACE_OUTER_BOUND('',#2517,.T.);
#1695=FACE_OUTER_BOUND('',#2518,.T.);
#1696=FACE_OUTER_BOUND('',#2519,.T.);
#1697=FACE_OUTER_BOUND('',#2521,.T.);
#1698=FACE_OUTER_BOUND('',#2522,.T.);
#1699=FACE_OUTER_BOUND('',#2523,.T.);
#1700=FACE_OUTER_BOUND('',#2524,.T.);
#1701=FACE_OUTER_BOUND('',#2527,.T.);
#1702=FACE_OUTER_BOUND('',#2529,.T.);
#1703=FACE_OUTER_BOUND('',#2530,.T.);
#1704=FACE_OUTER_BOUND('',#2532,.T.);
#1705=FACE_OUTER_BOUND('',#2533,.T.);
#1706=FACE_OUTER_BOUND('',#2535,.T.);
#1707=FACE_OUTER_BOUND('',#2536,.T.);
#1708=FACE_OUTER_BOUND('',#2538,.T.);
#1709=FACE_OUTER_BOUND('',#2539,.T.);
#1710=FACE_OUTER_BOUND('',#2541,.T.);
#1711=FACE_OUTER_BOUND('',#2542,.T.);
#1712=FACE_OUTER_BOUND('',#2543,.T.);
#1713=FACE_OUTER_BOUND('',#2544,.T.);
#1714=FACE_OUTER_BOUND('',#2545,.T.);
#1715=FACE_OUTER_BOUND('',#2546,.T.);
#1716=FACE_OUTER_BOUND('',#2547,.T.);
#1717=FACE_OUTER_BOUND('',#2548,.T.);
#1718=FACE_OUTER_BOUND('',#2549,.T.);
#1719=FACE_OUTER_BOUND('',#2554,.T.);
#1720=FACE_OUTER_BOUND('',#2555,.T.);
#1721=FACE_OUTER_BOUND('',#2556,.T.);
#1722=FACE_OUTER_BOUND('',#2557,.T.);
#1723=FACE_OUTER_BOUND('',#2558,.T.);
#1724=FACE_OUTER_BOUND('',#2559,.T.);
#1725=FACE_OUTER_BOUND('',#2564,.T.);
#1726=FACE_OUTER_BOUND('',#2565,.T.);
#1727=FACE_OUTER_BOUND('',#2566,.T.);
#1728=FACE_OUTER_BOUND('',#2567,.T.);
#1729=FACE_OUTER_BOUND('',#2568,.T.);
#1730=FACE_OUTER_BOUND('',#2569,.T.);
#1731=FACE_OUTER_BOUND('',#2570,.T.);
#1732=FACE_OUTER_BOUND('',#2571,.T.);
#1733=FACE_OUTER_BOUND('',#2573,.T.);
#1734=FACE_OUTER_BOUND('',#2574,.T.);
#1735=FACE_OUTER_BOUND('',#2576,.T.);
#1736=FACE_OUTER_BOUND('',#2577,.T.);
#1737=FACE_OUTER_BOUND('',#2578,.T.);
#1738=FACE_OUTER_BOUND('',#2579,.T.);
#1739=FACE_OUTER_BOUND('',#2581,.T.);
#1740=FACE_OUTER_BOUND('',#2582,.T.);
#1741=FACE_OUTER_BOUND('',#2583,.T.);
#1742=FACE_OUTER_BOUND('',#2584,.T.);
#1743=FACE_OUTER_BOUND('',#2586,.T.);
#1744=FACE_OUTER_BOUND('',#2587,.T.);
#1745=FACE_OUTER_BOUND('',#2588,.T.);
#1746=FACE_OUTER_BOUND('',#2589,.T.);
#1747=FACE_OUTER_BOUND('',#2590,.T.);
#1748=FACE_OUTER_BOUND('',#2591,.T.);
#1749=FACE_OUTER_BOUND('',#2592,.T.);
#1750=FACE_OUTER_BOUND('',#2593,.T.);
#1751=FACE_OUTER_BOUND('',#2594,.T.);
#1752=FACE_OUTER_BOUND('',#2595,.T.);
#1753=FACE_OUTER_BOUND('',#2596,.T.);
#1754=FACE_OUTER_BOUND('',#2597,.T.);
#1755=FACE_OUTER_BOUND('',#2598,.T.);
#1756=FACE_OUTER_BOUND('',#2599,.T.);
#1757=FACE_OUTER_BOUND('',#2600,.T.);
#1758=FACE_OUTER_BOUND('',#2601,.T.);
#1759=FACE_OUTER_BOUND('',#2602,.T.);
#1760=FACE_OUTER_BOUND('',#2603,.T.);
#1761=FACE_OUTER_BOUND('',#2604,.T.);
#1762=FACE_OUTER_BOUND('',#2605,.T.);
#1763=FACE_OUTER_BOUND('',#2606,.T.);
#1764=FACE_OUTER_BOUND('',#2607,.T.);
#1765=FACE_OUTER_BOUND('',#2608,.T.);
#1766=FACE_OUTER_BOUND('',#2609,.T.);
#1767=FACE_OUTER_BOUND('',#2611,.T.);
#1768=FACE_OUTER_BOUND('',#2612,.T.);
#1769=FACE_OUTER_BOUND('',#2614,.T.);
#1770=FACE_OUTER_BOUND('',#2615,.T.);
#1771=FACE_OUTER_BOUND('',#2617,.T.);
#1772=FACE_OUTER_BOUND('',#2618,.T.);
#1773=FACE_OUTER_BOUND('',#2620,.T.);
#1774=FACE_OUTER_BOUND('',#2621,.T.);
#1775=FACE_OUTER_BOUND('',#2623,.T.);
#1776=FACE_OUTER_BOUND('',#2624,.T.);
#1777=FACE_OUTER_BOUND('',#2625,.T.);
#1778=FACE_OUTER_BOUND('',#2626,.T.);
#1779=FACE_OUTER_BOUND('',#2627,.T.);
#1780=FACE_OUTER_BOUND('',#2628,.T.);
#1781=FACE_OUTER_BOUND('',#2630,.T.);
#1782=FACE_OUTER_BOUND('',#2631,.T.);
#1783=FACE_OUTER_BOUND('',#2633,.T.);
#1784=FACE_OUTER_BOUND('',#2634,.T.);
#1785=FACE_OUTER_BOUND('',#2635,.T.);
#1786=FACE_OUTER_BOUND('',#2636,.T.);
#1787=FACE_OUTER_BOUND('',#2638,.T.);
#1788=FACE_OUTER_BOUND('',#2639,.T.);
#1789=FACE_OUTER_BOUND('',#2640,.T.);
#1790=FACE_OUTER_BOUND('',#2641,.T.);
#1791=FACE_OUTER_BOUND('',#2643,.T.);
#1792=FACE_OUTER_BOUND('',#2644,.T.);
#1793=FACE_OUTER_BOUND('',#2645,.T.);
#1794=FACE_OUTER_BOUND('',#2646,.T.);
#1795=FACE_OUTER_BOUND('',#2647,.T.);
#1796=FACE_OUTER_BOUND('',#2648,.T.);
#1797=FACE_OUTER_BOUND('',#2649,.T.);
#1798=FACE_OUTER_BOUND('',#2650,.T.);
#1799=FACE_OUTER_BOUND('',#2651,.T.);
#1800=FACE_OUTER_BOUND('',#2652,.T.);
#1801=FACE_OUTER_BOUND('',#2653,.T.);
#1802=FACE_OUTER_BOUND('',#2654,.T.);
#1803=FACE_OUTER_BOUND('',#2655,.T.);
#1804=FACE_OUTER_BOUND('',#2656,.T.);
#1805=FACE_OUTER_BOUND('',#2657,.T.);
#1806=FACE_OUTER_BOUND('',#2658,.T.);
#1807=FACE_OUTER_BOUND('',#2659,.T.);
#1808=FACE_OUTER_BOUND('',#2660,.T.);
#1809=FACE_OUTER_BOUND('',#2661,.T.);
#1810=FACE_OUTER_BOUND('',#2662,.T.);
#1811=FACE_OUTER_BOUND('',#2663,.T.);
#1812=FACE_OUTER_BOUND('',#2664,.T.);
#1813=FACE_OUTER_BOUND('',#2665,.T.);
#1814=FACE_OUTER_BOUND('',#2666,.T.);
#1815=FACE_OUTER_BOUND('',#2667,.T.);
#1816=FACE_OUTER_BOUND('',#2668,.T.);
#1817=FACE_OUTER_BOUND('',#2669,.T.);
#1818=FACE_OUTER_BOUND('',#2671,.T.);
#1819=FACE_OUTER_BOUND('',#2672,.T.);
#1820=FACE_OUTER_BOUND('',#2674,.T.);
#1821=FACE_OUTER_BOUND('',#2675,.T.);
#1822=FACE_OUTER_BOUND('',#2677,.T.);
#1823=FACE_OUTER_BOUND('',#2678,.T.);
#1824=FACE_OUTER_BOUND('',#2680,.T.);
#1825=FACE_OUTER_BOUND('',#2681,.T.);
#1826=FACE_OUTER_BOUND('',#2683,.T.);
#1827=FACE_OUTER_BOUND('',#2684,.T.);
#1828=FACE_OUTER_BOUND('',#2685,.T.);
#1829=FACE_OUTER_BOUND('',#2686,.T.);
#1830=FACE_OUTER_BOUND('',#2687,.T.);
#1831=FACE_OUTER_BOUND('',#2688,.T.);
#1832=FACE_OUTER_BOUND('',#2689,.T.);
#1833=FACE_OUTER_BOUND('',#2690,.T.);
#1834=FACE_OUTER_BOUND('',#2691,.T.);
#1835=FACE_OUTER_BOUND('',#2692,.T.);
#1836=FACE_OUTER_BOUND('',#2693,.T.);
#1837=FACE_OUTER_BOUND('',#2694,.T.);
#1838=FACE_OUTER_BOUND('',#2695,.T.);
#1839=FACE_OUTER_BOUND('',#2696,.T.);
#1840=FACE_OUTER_BOUND('',#2697,.T.);
#1841=FACE_OUTER_BOUND('',#2698,.T.);
#1842=FACE_OUTER_BOUND('',#2699,.T.);
#1843=FACE_OUTER_BOUND('',#2700,.T.);
#1844=FACE_OUTER_BOUND('',#2701,.T.);
#1845=FACE_OUTER_BOUND('',#2702,.T.);
#1846=FACE_OUTER_BOUND('',#2703,.T.);
#1847=FACE_OUTER_BOUND('',#2704,.T.);
#1848=FACE_OUTER_BOUND('',#2705,.T.);
#1849=FACE_OUTER_BOUND('',#2706,.T.);
#1850=FACE_OUTER_BOUND('',#2707,.T.);
#1851=FACE_OUTER_BOUND('',#2708,.T.);
#1852=FACE_OUTER_BOUND('',#2709,.T.);
#1853=FACE_OUTER_BOUND('',#2710,.T.);
#1854=FACE_OUTER_BOUND('',#2711,.T.);
#1855=FACE_OUTER_BOUND('',#2712,.T.);
#1856=FACE_OUTER_BOUND('',#2713,.T.);
#1857=FACE_OUTER_BOUND('',#2714,.T.);
#1858=FACE_OUTER_BOUND('',#2715,.T.);
#1859=FACE_OUTER_BOUND('',#2716,.T.);
#1860=FACE_OUTER_BOUND('',#2717,.T.);
#1861=FACE_OUTER_BOUND('',#2718,.T.);
#1862=FACE_OUTER_BOUND('',#2719,.T.);
#1863=FACE_OUTER_BOUND('',#2720,.T.);
#1864=FACE_OUTER_BOUND('',#2721,.T.);
#1865=FACE_OUTER_BOUND('',#2722,.T.);
#1866=FACE_OUTER_BOUND('',#2723,.T.);
#1867=FACE_OUTER_BOUND('',#2724,.T.);
#1868=FACE_OUTER_BOUND('',#2725,.T.);
#1869=FACE_OUTER_BOUND('',#2726,.T.);
#1870=FACE_OUTER_BOUND('',#2727,.T.);
#1871=FACE_OUTER_BOUND('',#2728,.T.);
#1872=FACE_OUTER_BOUND('',#2729,.T.);
#1873=FACE_OUTER_BOUND('',#2731,.T.);
#1874=FACE_OUTER_BOUND('',#2733,.T.);
#1875=FACE_OUTER_BOUND('',#2734,.T.);
#1876=FACE_OUTER_BOUND('',#2735,.T.);
#1877=FACE_OUTER_BOUND('',#2736,.T.);
#1878=FACE_OUTER_BOUND('',#2737,.T.);
#1879=FACE_OUTER_BOUND('',#2738,.T.);
#1880=FACE_OUTER_BOUND('',#2739,.T.);
#1881=FACE_OUTER_BOUND('',#2740,.T.);
#1882=FACE_OUTER_BOUND('',#2741,.T.);
#1883=FACE_OUTER_BOUND('',#2742,.T.);
#1884=FACE_OUTER_BOUND('',#2744,.T.);
#1885=FACE_OUTER_BOUND('',#2745,.T.);
#1886=FACE_OUTER_BOUND('',#2746,.T.);
#1887=FACE_OUTER_BOUND('',#2748,.T.);
#1888=FACE_OUTER_BOUND('',#2749,.T.);
#1889=FACE_OUTER_BOUND('',#2751,.T.);
#1890=FACE_OUTER_BOUND('',#2752,.T.);
#1891=FACE_OUTER_BOUND('',#2753,.T.);
#1892=FACE_OUTER_BOUND('',#2754,.T.);
#1893=FACE_OUTER_BOUND('',#2755,.T.);
#1894=FACE_OUTER_BOUND('',#2756,.T.);
#1895=FACE_OUTER_BOUND('',#2757,.T.);
#1896=FACE_OUTER_BOUND('',#2758,.T.);
#1897=FACE_OUTER_BOUND('',#2759,.T.);
#1898=FACE_OUTER_BOUND('',#2760,.T.);
#1899=FACE_OUTER_BOUND('',#2761,.T.);
#1900=FACE_OUTER_BOUND('',#2762,.T.);
#1901=FACE_OUTER_BOUND('',#2763,.T.);
#1902=FACE_OUTER_BOUND('',#2764,.T.);
#1903=FACE_OUTER_BOUND('',#2766,.T.);
#1904=FACE_OUTER_BOUND('',#2767,.T.);
#1905=FACE_OUTER_BOUND('',#2768,.T.);
#1906=FACE_OUTER_BOUND('',#2769,.T.);
#1907=FACE_OUTER_BOUND('',#2770,.T.);
#1908=FACE_OUTER_BOUND('',#2771,.T.);
#1909=FACE_OUTER_BOUND('',#2772,.T.);
#1910=FACE_OUTER_BOUND('',#2773,.T.);
#1911=FACE_OUTER_BOUND('',#2774,.T.);
#1912=FACE_OUTER_BOUND('',#2775,.T.);
#1913=FACE_OUTER_BOUND('',#2776,.T.);
#1914=FACE_OUTER_BOUND('',#2781,.T.);
#1915=FACE_OUTER_BOUND('',#2786,.T.);
#1916=FACE_OUTER_BOUND('',#2787,.T.);
#1917=FACE_OUTER_BOUND('',#2788,.T.);
#1918=FACE_OUTER_BOUND('',#2789,.T.);
#1919=FACE_OUTER_BOUND('',#2790,.T.);
#1920=FACE_OUTER_BOUND('',#2791,.T.);
#1921=FACE_OUTER_BOUND('',#2792,.T.);
#1922=FACE_OUTER_BOUND('',#2793,.T.);
#1923=FACE_OUTER_BOUND('',#2794,.T.);
#1924=FACE_OUTER_BOUND('',#2795,.T.);
#1925=FACE_OUTER_BOUND('',#2796,.T.);
#1926=FACE_OUTER_BOUND('',#2797,.T.);
#1927=FACE_OUTER_BOUND('',#2798,.T.);
#1928=FACE_OUTER_BOUND('',#2807,.T.);
#1929=FACE_OUTER_BOUND('',#2816,.T.);
#1930=FACE_OUTER_BOUND('',#2817,.T.);
#1931=FACE_OUTER_BOUND('',#2818,.T.);
#1932=FACE_OUTER_BOUND('',#2819,.T.);
#1933=FACE_OUTER_BOUND('',#2820,.T.);
#1934=FACE_OUTER_BOUND('',#2821,.T.);
#1935=FACE_OUTER_BOUND('',#2822,.T.);
#1936=FACE_OUTER_BOUND('',#2823,.T.);
#1937=FACE_OUTER_BOUND('',#2824,.T.);
#1938=FACE_OUTER_BOUND('',#2825,.T.);
#1939=FACE_OUTER_BOUND('',#2826,.T.);
#1940=FACE_OUTER_BOUND('',#2827,.T.);
#1941=FACE_OUTER_BOUND('',#2828,.T.);
#1942=FACE_OUTER_BOUND('',#2829,.T.);
#1943=FACE_OUTER_BOUND('',#2830,.T.);
#1944=FACE_OUTER_BOUND('',#2831,.T.);
#1945=FACE_OUTER_BOUND('',#2832,.T.);
#1946=FACE_OUTER_BOUND('',#2837,.T.);
#1947=FACE_OUTER_BOUND('',#2838,.T.);
#1948=FACE_OUTER_BOUND('',#2840,.T.);
#1949=FACE_OUTER_BOUND('',#2845,.T.);
#1950=FACE_OUTER_BOUND('',#2846,.T.);
#1951=FACE_OUTER_BOUND('',#2847,.T.);
#1952=FACE_OUTER_BOUND('',#2848,.T.);
#1953=FACE_OUTER_BOUND('',#2849,.T.);
#1954=FACE_OUTER_BOUND('',#2850,.T.);
#1955=FACE_OUTER_BOUND('',#2851,.T.);
#1956=FACE_OUTER_BOUND('',#2852,.T.);
#1957=FACE_OUTER_BOUND('',#2853,.T.);
#1958=FACE_OUTER_BOUND('',#2854,.T.);
#1959=FACE_OUTER_BOUND('',#2855,.T.);
#1960=FACE_OUTER_BOUND('',#2856,.T.);
#1961=FACE_OUTER_BOUND('',#2857,.T.);
#1962=FACE_OUTER_BOUND('',#2858,.T.);
#1963=FACE_OUTER_BOUND('',#2859,.T.);
#1964=FACE_OUTER_BOUND('',#2864,.T.);
#1965=FACE_OUTER_BOUND('',#2865,.T.);
#1966=FACE_OUTER_BOUND('',#2866,.T.);
#1967=FACE_OUTER_BOUND('',#2867,.T.);
#1968=FACE_OUTER_BOUND('',#2868,.T.);
#1969=FACE_OUTER_BOUND('',#2869,.T.);
#1970=FACE_OUTER_BOUND('',#2870,.T.);
#1971=FACE_OUTER_BOUND('',#2871,.T.);
#1972=FACE_OUTER_BOUND('',#2872,.T.);
#1973=FACE_OUTER_BOUND('',#2873,.T.);
#1974=FACE_OUTER_BOUND('',#2874,.T.);
#1975=FACE_OUTER_BOUND('',#2875,.T.);
#1976=FACE_OUTER_BOUND('',#2876,.T.);
#1977=FACE_OUTER_BOUND('',#2877,.T.);
#1978=FACE_OUTER_BOUND('',#2878,.T.);
#1979=FACE_OUTER_BOUND('',#2879,.T.);
#1980=FACE_OUTER_BOUND('',#2880,.T.);
#1981=FACE_OUTER_BOUND('',#2881,.T.);
#1982=FACE_OUTER_BOUND('',#2882,.T.);
#1983=FACE_OUTER_BOUND('',#2883,.T.);
#1984=FACE_OUTER_BOUND('',#2884,.T.);
#1985=FACE_OUTER_BOUND('',#2885,.T.);
#1986=FACE_OUTER_BOUND('',#2886,.T.);
#1987=FACE_OUTER_BOUND('',#2887,.T.);
#1988=FACE_OUTER_BOUND('',#2888,.T.);
#1989=FACE_OUTER_BOUND('',#2889,.T.);
#1990=FACE_OUTER_BOUND('',#2890,.T.);
#1991=FACE_OUTER_BOUND('',#2891,.T.);
#1992=FACE_OUTER_BOUND('',#2892,.T.);
#1993=FACE_OUTER_BOUND('',#2893,.T.);
#1994=FACE_OUTER_BOUND('',#2894,.T.);
#1995=FACE_OUTER_BOUND('',#2896,.T.);
#1996=FACE_OUTER_BOUND('',#2897,.T.);
#1997=FACE_OUTER_BOUND('',#2899,.T.);
#1998=FACE_OUTER_BOUND('',#2900,.T.);
#1999=FACE_OUTER_BOUND('',#2901,.T.);
#2000=FACE_OUTER_BOUND('',#2902,.T.);
#2001=FACE_OUTER_BOUND('',#2903,.T.);
#2002=FACE_OUTER_BOUND('',#2904,.T.);
#2003=FACE_OUTER_BOUND('',#2905,.T.);
#2004=FACE_OUTER_BOUND('',#2906,.T.);
#2005=FACE_OUTER_BOUND('',#2907,.T.);
#2006=FACE_OUTER_BOUND('',#2909,.T.);
#2007=FACE_OUTER_BOUND('',#2910,.T.);
#2008=FACE_OUTER_BOUND('',#2911,.T.);
#2009=FACE_OUTER_BOUND('',#2912,.T.);
#2010=FACE_OUTER_BOUND('',#2913,.T.);
#2011=FACE_OUTER_BOUND('',#2914,.T.);
#2012=FACE_OUTER_BOUND('',#2915,.T.);
#2013=FACE_OUTER_BOUND('',#2917,.T.);
#2014=FACE_OUTER_BOUND('',#2918,.T.);
#2015=FACE_OUTER_BOUND('',#2919,.T.);
#2016=FACE_OUTER_BOUND('',#2920,.T.);
#2017=FACE_OUTER_BOUND('',#2921,.T.);
#2018=FACE_OUTER_BOUND('',#2922,.T.);
#2019=FACE_OUTER_BOUND('',#2923,.T.);
#2020=FACE_OUTER_BOUND('',#2924,.T.);
#2021=FACE_OUTER_BOUND('',#2925,.T.);
#2022=FACE_OUTER_BOUND('',#2926,.T.);
#2023=FACE_OUTER_BOUND('',#2927,.T.);
#2024=FACE_OUTER_BOUND('',#2928,.T.);
#2025=FACE_OUTER_BOUND('',#2929,.T.);
#2026=FACE_OUTER_BOUND('',#2930,.T.);
#2027=FACE_OUTER_BOUND('',#2931,.T.);
#2028=FACE_OUTER_BOUND('',#2932,.T.);
#2029=FACE_OUTER_BOUND('',#2933,.T.);
#2030=FACE_OUTER_BOUND('',#2934,.T.);
#2031=FACE_OUTER_BOUND('',#2935,.T.);
#2032=FACE_OUTER_BOUND('',#2936,.T.);
#2033=FACE_OUTER_BOUND('',#2937,.T.);
#2034=FACE_OUTER_BOUND('',#2938,.T.);
#2035=FACE_OUTER_BOUND('',#2939,.T.);
#2036=FACE_OUTER_BOUND('',#2940,.T.);
#2037=FACE_OUTER_BOUND('',#2945,.T.);
#2038=FACE_OUTER_BOUND('',#2946,.T.);
#2039=FACE_OUTER_BOUND('',#2947,.T.);
#2040=FACE_OUTER_BOUND('',#2948,.T.);
#2041=FACE_OUTER_BOUND('',#2949,.T.);
#2042=FACE_OUTER_BOUND('',#2954,.T.);
#2043=FACE_OUTER_BOUND('',#2955,.T.);
#2044=FACE_OUTER_BOUND('',#2956,.T.);
#2045=FACE_OUTER_BOUND('',#2957,.T.);
#2046=FACE_OUTER_BOUND('',#2959,.T.);
#2047=FACE_OUTER_BOUND('',#2960,.T.);
#2048=FACE_OUTER_BOUND('',#2961,.T.);
#2049=FACE_OUTER_BOUND('',#2962,.T.);
#2050=FACE_OUTER_BOUND('',#2963,.T.);
#2051=FACE_OUTER_BOUND('',#2965,.T.);
#2052=FACE_OUTER_BOUND('',#2966,.T.);
#2053=FACE_OUTER_BOUND('',#2967,.T.);
#2054=FACE_OUTER_BOUND('',#2968,.T.);
#2055=FACE_OUTER_BOUND('',#2969,.T.);
#2056=FACE_OUTER_BOUND('',#2970,.T.);
#2057=FACE_OUTER_BOUND('',#2971,.T.);
#2058=FACE_OUTER_BOUND('',#2972,.T.);
#2059=FACE_OUTER_BOUND('',#2973,.T.);
#2060=FACE_OUTER_BOUND('',#2974,.T.);
#2061=FACE_OUTER_BOUND('',#2975,.T.);
#2062=FACE_OUTER_BOUND('',#2976,.T.);
#2063=FACE_OUTER_BOUND('',#2977,.T.);
#2064=FACE_OUTER_BOUND('',#2978,.T.);
#2065=FACE_OUTER_BOUND('',#2979,.T.);
#2066=FACE_OUTER_BOUND('',#2980,.T.);
#2067=FACE_OUTER_BOUND('',#2981,.T.);
#2068=FACE_OUTER_BOUND('',#2983,.T.);
#2069=FACE_OUTER_BOUND('',#2984,.T.);
#2070=FACE_OUTER_BOUND('',#2985,.T.);
#2071=FACE_OUTER_BOUND('',#2986,.T.);
#2072=FACE_OUTER_BOUND('',#2987,.T.);
#2073=FACE_OUTER_BOUND('',#2988,.T.);
#2074=FACE_OUTER_BOUND('',#2989,.T.);
#2075=FACE_OUTER_BOUND('',#2990,.T.);
#2076=FACE_OUTER_BOUND('',#2991,.T.);
#2077=FACE_OUTER_BOUND('',#2992,.T.);
#2078=FACE_OUTER_BOUND('',#2993,.T.);
#2079=FACE_OUTER_BOUND('',#2994,.T.);
#2080=FACE_OUTER_BOUND('',#2995,.T.);
#2081=FACE_OUTER_BOUND('',#2996,.T.);
#2082=FACE_OUTER_BOUND('',#2997,.T.);
#2083=FACE_OUTER_BOUND('',#2998,.T.);
#2084=FACE_OUTER_BOUND('',#2999,.T.);
#2085=FACE_OUTER_BOUND('',#3000,.T.);
#2086=FACE_OUTER_BOUND('',#3001,.T.);
#2087=FACE_OUTER_BOUND('',#3002,.T.);
#2088=FACE_OUTER_BOUND('',#3003,.T.);
#2089=FACE_OUTER_BOUND('',#3004,.T.);
#2090=FACE_OUTER_BOUND('',#3005,.T.);
#2091=FACE_OUTER_BOUND('',#3006,.T.);
#2092=FACE_OUTER_BOUND('',#3007,.T.);
#2093=FACE_OUTER_BOUND('',#3008,.T.);
#2094=FACE_OUTER_BOUND('',#3009,.T.);
#2095=FACE_OUTER_BOUND('',#3010,.T.);
#2096=FACE_OUTER_BOUND('',#3011,.T.);
#2097=FACE_OUTER_BOUND('',#3012,.T.);
#2098=FACE_OUTER_BOUND('',#3013,.T.);
#2099=FACE_OUTER_BOUND('',#3014,.T.);
#2100=FACE_OUTER_BOUND('',#3015,.T.);
#2101=FACE_OUTER_BOUND('',#3016,.T.);
#2102=FACE_OUTER_BOUND('',#3017,.T.);
#2103=FACE_OUTER_BOUND('',#3018,.T.);
#2104=FACE_OUTER_BOUND('',#3019,.T.);
#2105=FACE_OUTER_BOUND('',#3020,.T.);
#2106=FACE_OUTER_BOUND('',#3021,.T.);
#2107=FACE_OUTER_BOUND('',#3022,.T.);
#2108=FACE_OUTER_BOUND('',#3023,.T.);
#2109=FACE_OUTER_BOUND('',#3024,.T.);
#2110=FACE_OUTER_BOUND('',#3025,.T.);
#2111=FACE_OUTER_BOUND('',#3026,.T.);
#2112=FACE_OUTER_BOUND('',#3027,.T.);
#2113=FACE_OUTER_BOUND('',#3028,.T.);
#2114=FACE_OUTER_BOUND('',#3029,.T.);
#2115=FACE_OUTER_BOUND('',#3030,.T.);
#2116=FACE_OUTER_BOUND('',#3031,.T.);
#2117=FACE_OUTER_BOUND('',#3032,.T.);
#2118=FACE_OUTER_BOUND('',#3033,.T.);
#2119=FACE_OUTER_BOUND('',#3034,.T.);
#2120=FACE_OUTER_BOUND('',#3035,.T.);
#2121=FACE_OUTER_BOUND('',#3036,.T.);
#2122=FACE_OUTER_BOUND('',#3037,.T.);
#2123=FACE_OUTER_BOUND('',#3038,.T.);
#2124=FACE_OUTER_BOUND('',#3039,.T.);
#2125=FACE_OUTER_BOUND('',#3040,.T.);
#2126=FACE_OUTER_BOUND('',#3041,.T.);
#2127=FACE_OUTER_BOUND('',#3042,.T.);
#2128=FACE_OUTER_BOUND('',#3043,.T.);
#2129=FACE_OUTER_BOUND('',#3044,.T.);
#2130=FACE_OUTER_BOUND('',#3045,.T.);
#2131=FACE_OUTER_BOUND('',#3046,.T.);
#2132=FACE_OUTER_BOUND('',#3047,.T.);
#2133=FACE_OUTER_BOUND('',#3048,.T.);
#2134=FACE_OUTER_BOUND('',#3049,.T.);
#2135=FACE_OUTER_BOUND('',#3050,.T.);
#2136=FACE_OUTER_BOUND('',#3051,.T.);
#2137=FACE_OUTER_BOUND('',#3052,.T.);
#2138=FACE_OUTER_BOUND('',#3053,.T.);
#2139=FACE_OUTER_BOUND('',#3054,.T.);
#2140=FACE_OUTER_BOUND('',#3055,.T.);
#2141=FACE_OUTER_BOUND('',#3056,.T.);
#2142=FACE_OUTER_BOUND('',#3057,.T.);
#2143=FACE_OUTER_BOUND('',#3058,.T.);
#2144=FACE_OUTER_BOUND('',#3059,.T.);
#2145=FACE_OUTER_BOUND('',#3060,.T.);
#2146=FACE_OUTER_BOUND('',#3061,.T.);
#2147=FACE_OUTER_BOUND('',#3062,.T.);
#2148=FACE_OUTER_BOUND('',#3063,.T.);
#2149=FACE_OUTER_BOUND('',#3064,.T.);
#2150=FACE_OUTER_BOUND('',#3065,.T.);
#2151=FACE_OUTER_BOUND('',#3066,.T.);
#2152=FACE_OUTER_BOUND('',#3067,.T.);
#2153=FACE_OUTER_BOUND('',#3068,.T.);
#2154=FACE_OUTER_BOUND('',#3069,.T.);
#2155=FACE_OUTER_BOUND('',#3070,.T.);
#2156=FACE_OUTER_BOUND('',#3071,.T.);
#2157=FACE_OUTER_BOUND('',#3072,.T.);
#2158=FACE_OUTER_BOUND('',#3073,.T.);
#2159=FACE_OUTER_BOUND('',#3074,.T.);
#2160=FACE_OUTER_BOUND('',#3075,.T.);
#2161=FACE_OUTER_BOUND('',#3076,.T.);
#2162=FACE_OUTER_BOUND('',#3077,.T.);
#2163=FACE_OUTER_BOUND('',#3078,.T.);
#2164=FACE_OUTER_BOUND('',#3079,.T.);
#2165=FACE_OUTER_BOUND('',#3080,.T.);
#2166=FACE_OUTER_BOUND('',#3081,.T.);
#2167=FACE_OUTER_BOUND('',#3082,.T.);
#2168=FACE_OUTER_BOUND('',#3083,.T.);
#2169=FACE_OUTER_BOUND('',#3084,.T.);
#2170=FACE_OUTER_BOUND('',#3085,.T.);
#2171=FACE_OUTER_BOUND('',#3086,.T.);
#2172=FACE_OUTER_BOUND('',#3087,.T.);
#2173=FACE_OUTER_BOUND('',#3088,.T.);
#2174=FACE_OUTER_BOUND('',#3089,.T.);
#2175=FACE_OUTER_BOUND('',#3090,.T.);
#2176=FACE_OUTER_BOUND('',#3091,.T.);
#2177=FACE_OUTER_BOUND('',#3092,.T.);
#2178=FACE_OUTER_BOUND('',#3093,.T.);
#2179=FACE_OUTER_BOUND('',#3094,.T.);
#2180=FACE_OUTER_BOUND('',#3095,.T.);
#2181=FACE_OUTER_BOUND('',#3096,.T.);
#2182=FACE_OUTER_BOUND('',#3097,.T.);
#2183=FACE_OUTER_BOUND('',#3098,.T.);
#2184=FACE_OUTER_BOUND('',#3099,.T.);
#2185=FACE_OUTER_BOUND('',#3100,.T.);
#2186=FACE_OUTER_BOUND('',#3101,.T.);
#2187=FACE_OUTER_BOUND('',#3102,.T.);
#2188=FACE_OUTER_BOUND('',#3103,.T.);
#2189=FACE_OUTER_BOUND('',#3104,.T.);
#2190=FACE_OUTER_BOUND('',#3105,.T.);
#2191=FACE_OUTER_BOUND('',#3106,.T.);
#2192=FACE_OUTER_BOUND('',#3107,.T.);
#2193=FACE_OUTER_BOUND('',#3108,.T.);
#2194=FACE_OUTER_BOUND('',#3109,.T.);
#2195=FACE_OUTER_BOUND('',#3110,.T.);
#2196=FACE_OUTER_BOUND('',#3111,.T.);
#2197=FACE_OUTER_BOUND('',#3112,.T.);
#2198=FACE_OUTER_BOUND('',#3113,.T.);
#2199=FACE_OUTER_BOUND('',#3114,.T.);
#2200=FACE_OUTER_BOUND('',#3115,.T.);
#2201=FACE_OUTER_BOUND('',#3116,.T.);
#2202=FACE_OUTER_BOUND('',#3117,.T.);
#2203=FACE_OUTER_BOUND('',#3118,.T.);
#2204=FACE_OUTER_BOUND('',#3119,.T.);
#2205=FACE_OUTER_BOUND('',#3120,.T.);
#2206=FACE_OUTER_BOUND('',#3121,.T.);
#2207=FACE_OUTER_BOUND('',#3123,.T.);
#2208=FACE_OUTER_BOUND('',#3124,.T.);
#2209=FACE_OUTER_BOUND('',#3125,.T.);
#2210=FACE_OUTER_BOUND('',#3126,.T.);
#2211=FACE_OUTER_BOUND('',#3127,.T.);
#2212=FACE_OUTER_BOUND('',#3128,.T.);
#2213=FACE_OUTER_BOUND('',#3129,.T.);
#2214=FACE_OUTER_BOUND('',#3130,.T.);
#2215=FACE_OUTER_BOUND('',#3131,.T.);
#2216=FACE_OUTER_BOUND('',#3132,.T.);
#2217=FACE_OUTER_BOUND('',#3133,.T.);
#2218=FACE_OUTER_BOUND('',#3135,.T.);
#2219=FACE_OUTER_BOUND('',#3136,.T.);
#2220=FACE_OUTER_BOUND('',#3138,.T.);
#2221=FACE_OUTER_BOUND('',#3139,.T.);
#2222=FACE_OUTER_BOUND('',#3141,.T.);
#2223=FACE_OUTER_BOUND('',#3142,.T.);
#2224=FACE_OUTER_BOUND('',#3143,.T.);
#2225=FACE_OUTER_BOUND('',#3144,.T.);
#2226=FACE_OUTER_BOUND('',#3146,.T.);
#2227=FACE_OUTER_BOUND('',#3148,.T.);
#2228=FACE_OUTER_BOUND('',#3149,.T.);
#2229=FACE_OUTER_BOUND('',#3150,.T.);
#2230=FACE_OUTER_BOUND('',#3151,.T.);
#2231=FACE_OUTER_BOUND('',#3153,.T.);
#2232=FACE_OUTER_BOUND('',#3155,.T.);
#2233=FACE_OUTER_BOUND('',#3157,.T.);
#2234=FACE_OUTER_BOUND('',#3159,.T.);
#2235=FACE_OUTER_BOUND('',#3160,.T.);
#2236=FACE_OUTER_BOUND('',#3161,.T.);
#2237=FACE_OUTER_BOUND('',#3162,.T.);
#2238=FACE_OUTER_BOUND('',#3163,.T.);
#2239=FACE_OUTER_BOUND('',#3164,.T.);
#2240=FACE_OUTER_BOUND('',#3165,.T.);
#2241=FACE_OUTER_BOUND('',#3166,.T.);
#2242=FACE_OUTER_BOUND('',#3169,.T.);
#2243=FACE_OUTER_BOUND('',#3172,.T.);
#2244=FACE_OUTER_BOUND('',#3173,.T.);
#2245=FACE_OUTER_BOUND('',#3175,.T.);
#2246=FACE_OUTER_BOUND('',#3177,.T.);
#2247=FACE_OUTER_BOUND('',#3178,.T.);
#2248=FACE_OUTER_BOUND('',#3179,.T.);
#2249=FACE_OUTER_BOUND('',#3180,.T.);
#2250=FACE_OUTER_BOUND('',#3182,.T.);
#2251=FACE_OUTER_BOUND('',#3184,.T.);
#2252=FACE_OUTER_BOUND('',#3185,.T.);
#2253=FACE_OUTER_BOUND('',#3186,.T.);
#2254=FACE_OUTER_BOUND('',#3188,.T.);
#2255=FACE_OUTER_BOUND('',#3190,.T.);
#2256=FACE_OUTER_BOUND('',#3191,.T.);
#2257=FACE_OUTER_BOUND('',#3192,.T.);
#2258=FACE_OUTER_BOUND('',#3193,.T.);
#2259=FACE_OUTER_BOUND('',#3194,.T.);
#2260=FACE_OUTER_BOUND('',#3195,.T.);
#2261=FACE_OUTER_BOUND('',#3196,.T.);
#2262=FACE_OUTER_BOUND('',#3197,.T.);
#2263=FACE_OUTER_BOUND('',#3198,.T.);
#2264=FACE_OUTER_BOUND('',#3199,.T.);
#2265=FACE_OUTER_BOUND('',#3200,.T.);
#2266=FACE_OUTER_BOUND('',#3201,.T.);
#2267=FACE_OUTER_BOUND('',#3202,.T.);
#2268=FACE_OUTER_BOUND('',#3203,.T.);
#2269=FACE_OUTER_BOUND('',#3204,.T.);
#2270=FACE_OUTER_BOUND('',#3205,.T.);
#2271=FACE_OUTER_BOUND('',#3206,.T.);
#2272=FACE_OUTER_BOUND('',#3207,.T.);
#2273=FACE_OUTER_BOUND('',#3209,.T.);
#2274=FACE_OUTER_BOUND('',#3210,.T.);
#2275=FACE_OUTER_BOUND('',#3211,.T.);
#2276=FACE_OUTER_BOUND('',#3212,.T.);
#2277=FACE_OUTER_BOUND('',#3213,.T.);
#2278=FACE_OUTER_BOUND('',#3214,.T.);
#2279=FACE_OUTER_BOUND('',#3215,.T.);
#2280=FACE_OUTER_BOUND('',#3217,.T.);
#2281=FACE_OUTER_BOUND('',#3219,.T.);
#2282=FACE_OUTER_BOUND('',#3220,.T.);
#2283=FACE_OUTER_BOUND('',#3221,.T.);
#2284=FACE_OUTER_BOUND('',#3222,.T.);
#2285=FACE_OUTER_BOUND('',#3223,.T.);
#2286=FACE_OUTER_BOUND('',#3225,.T.);
#2287=FACE_OUTER_BOUND('',#3226,.T.);
#2288=FACE_OUTER_BOUND('',#3227,.T.);
#2289=FACE_OUTER_BOUND('',#3228,.T.);
#2290=FACE_OUTER_BOUND('',#3229,.T.);
#2291=FACE_OUTER_BOUND('',#3230,.T.);
#2292=FACE_OUTER_BOUND('',#3231,.T.);
#2293=FACE_OUTER_BOUND('',#3232,.T.);
#2294=FACE_OUTER_BOUND('',#3233,.T.);
#2295=FACE_OUTER_BOUND('',#3234,.T.);
#2296=FACE_OUTER_BOUND('',#3235,.T.);
#2297=FACE_OUTER_BOUND('',#3236,.T.);
#2298=EDGE_LOOP('',(#8489,#8490,#8491,#8492));
#2299=EDGE_LOOP('',(#8493,#8494,#8495,#8496));
#2300=EDGE_LOOP('',(#8497,#8498,#8499,#8500));
#2301=EDGE_LOOP('',(#8501,#8502,#8503,#8504));
#2302=EDGE_LOOP('',(#8505,#8506,#8507,#8508));
#2303=EDGE_LOOP('',(#8509,#8510,#8511,#8512));
#2304=EDGE_LOOP('',(#8513,#8514,#8515,#8516));
#2305=EDGE_LOOP('',(#8517,#8518,#8519,#8520));
#2306=EDGE_LOOP('',(#8521,#8522,#8523,#8524));
#2307=EDGE_LOOP('',(#8525,#8526,#8527,#8528));
#2308=EDGE_LOOP('',(#8529,#8530,#8531,#8532));
#2309=EDGE_LOOP('',(#8533,#8534,#8535,#8536));
#2310=EDGE_LOOP('',(#8537,#8538,#8539,#8540));
#2311=EDGE_LOOP('',(#8541,#8542,#8543,#8544));
#2312=EDGE_LOOP('',(#8545,#8546,#8547,#8548));
#2313=EDGE_LOOP('',(#8549,#8550,#8551,#8552));
#2314=EDGE_LOOP('',(#8553,#8554,#8555,#8556));
#2315=EDGE_LOOP('',(#8557,#8558,#8559,#8560));
#2316=EDGE_LOOP('',(#8561,#8562,#8563,#8564));
#2317=EDGE_LOOP('',(#8565,#8566,#8567,#8568));
#2318=EDGE_LOOP('',(#8569,#8570,#8571,#8572));
#2319=EDGE_LOOP('',(#8573));
#2320=EDGE_LOOP('',(#8574));
#2321=EDGE_LOOP('',(#8575));
#2322=EDGE_LOOP('',(#8576));
#2323=EDGE_LOOP('',(#8577));
#2324=EDGE_LOOP('',(#8578));
#2325=EDGE_LOOP('',(#8579));
#2326=EDGE_LOOP('',(#8580));
#2327=EDGE_LOOP('',(#8581));
#2328=EDGE_LOOP('',(#8582));
#2329=EDGE_LOOP('',(#8583));
#2330=EDGE_LOOP('',(#8584));
#2331=EDGE_LOOP('',(#8585));
#2332=EDGE_LOOP('',(#8586));
#2333=EDGE_LOOP('',(#8587));
#2334=EDGE_LOOP('',(#8588));
#2335=EDGE_LOOP('',(#8589,#8590,#8591,#8592));
#2336=EDGE_LOOP('',(#8593));
#2337=EDGE_LOOP('',(#8594));
#2338=EDGE_LOOP('',(#8595));
#2339=EDGE_LOOP('',(#8596));
#2340=EDGE_LOOP('',(#8597));
#2341=EDGE_LOOP('',(#8598));
#2342=EDGE_LOOP('',(#8599));
#2343=EDGE_LOOP('',(#8600));
#2344=EDGE_LOOP('',(#8601));
#2345=EDGE_LOOP('',(#8602));
#2346=EDGE_LOOP('',(#8603));
#2347=EDGE_LOOP('',(#8604));
#2348=EDGE_LOOP('',(#8605));
#2349=EDGE_LOOP('',(#8606));
#2350=EDGE_LOOP('',(#8607));
#2351=EDGE_LOOP('',(#8608));
#2352=EDGE_LOOP('',(#8609,#8610,#8611,#8612));
#2353=EDGE_LOOP('',(#8613,#8614,#8615,#8616));
#2354=EDGE_LOOP('',(#8617,#8618,#8619,#8620));
#2355=EDGE_LOOP('',(#8621,#8622,#8623,#8624));
#2356=EDGE_LOOP('',(#8625,#8626,#8627,#8628));
#2357=EDGE_LOOP('',(#8629));
#2358=EDGE_LOOP('',(#8630));
#2359=EDGE_LOOP('',(#8631,#8632,#8633,#8634));
#2360=EDGE_LOOP('',(#8635));
#2361=EDGE_LOOP('',(#8636));
#2362=EDGE_LOOP('',(#8637,#8638,#8639,#8640));
#2363=EDGE_LOOP('',(#8641));
#2364=EDGE_LOOP('',(#8642));
#2365=EDGE_LOOP('',(#8643,#8644,#8645,#8646));
#2366=EDGE_LOOP('',(#8647));
#2367=EDGE_LOOP('',(#8648));
#2368=EDGE_LOOP('',(#8649,#8650,#8651,#8652));
#2369=EDGE_LOOP('',(#8653,#8654,#8655,#8656));
#2370=EDGE_LOOP('',(#8657,#8658,#8659,#8660));
#2371=EDGE_LOOP('',(#8661,#8662,#8663,#8664));
#2372=EDGE_LOOP('',(#8665,#8666,#8667,#8668));
#2373=EDGE_LOOP('',(#8669,#8670,#8671,#8672));
#2374=EDGE_LOOP('',(#8673,#8674,#8675,#8676));
#2375=EDGE_LOOP('',(#8677,#8678,#8679,#8680));
#2376=EDGE_LOOP('',(#8681,#8682,#8683,#8684));
#2377=EDGE_LOOP('',(#8685));
#2378=EDGE_LOOP('',(#8686));
#2379=EDGE_LOOP('',(#8687));
#2380=EDGE_LOOP('',(#8688));
#2381=EDGE_LOOP('',(#8689));
#2382=EDGE_LOOP('',(#8690));
#2383=EDGE_LOOP('',(#8691));
#2384=EDGE_LOOP('',(#8692));
#2385=EDGE_LOOP('',(#8693,#8694,#8695,#8696));
#2386=EDGE_LOOP('',(#8697));
#2387=EDGE_LOOP('',(#8698));
#2388=EDGE_LOOP('',(#8699));
#2389=EDGE_LOOP('',(#8700));
#2390=EDGE_LOOP('',(#8701));
#2391=EDGE_LOOP('',(#8702));
#2392=EDGE_LOOP('',(#8703));
#2393=EDGE_LOOP('',(#8704));
#2394=EDGE_LOOP('',(#8705,#8706,#8707,#8708));
#2395=EDGE_LOOP('',(#8709,#8710,#8711,#8712));
#2396=EDGE_LOOP('',(#8713,#8714,#8715,#8716));
#2397=EDGE_LOOP('',(#8717,#8718,#8719,#8720));
#2398=EDGE_LOOP('',(#8721));
#2399=EDGE_LOOP('',(#8722));
#2400=EDGE_LOOP('',(#8723,#8724,#8725,#8726));
#2401=EDGE_LOOP('',(#8727,#8728,#8729,#8730));
#2402=EDGE_LOOP('',(#8731));
#2403=EDGE_LOOP('',(#8732,#8733,#8734,#8735));
#2404=EDGE_LOOP('',(#8736));
#2405=EDGE_LOOP('',(#8737,#8738,#8739,#8740));
#2406=EDGE_LOOP('',(#8741,#8742,#8743,#8744));
#2407=EDGE_LOOP('',(#8745));
#2408=EDGE_LOOP('',(#8746));
#2409=EDGE_LOOP('',(#8747));
#2410=EDGE_LOOP('',(#8748));
#2411=EDGE_LOOP('',(#8749,#8750,#8751,#8752));
#2412=EDGE_LOOP('',(#8753,#8754,#8755,#8756));
#2413=EDGE_LOOP('',(#8757));
#2414=EDGE_LOOP('',(#8758));
#2415=EDGE_LOOP('',(#8759));
#2416=EDGE_LOOP('',(#8760));
#2417=EDGE_LOOP('',(#8761,#8762,#8763,#8764));
#2418=EDGE_LOOP('',(#8765,#8766,#8767,#8768));
#2419=EDGE_LOOP('',(#8769));
#2420=EDGE_LOOP('',(#8770));
#2421=EDGE_LOOP('',(#8771,#8772,#8773,#8774));
#2422=EDGE_LOOP('',(#8775,#8776,#8777,#8778));
#2423=EDGE_LOOP('',(#8779,#8780,#8781,#8782));
#2424=EDGE_LOOP('',(#8783,#8784,#8785,#8786));
#2425=EDGE_LOOP('',(#8787));
#2426=EDGE_LOOP('',(#8788));
#2427=EDGE_LOOP('',(#8789,#8790,#8791,#8792));
#2428=EDGE_LOOP('',(#8793,#8794,#8795,#8796));
#2429=EDGE_LOOP('',(#8797));
#2430=EDGE_LOOP('',(#8798));
#2431=EDGE_LOOP('',(#8799));
#2432=EDGE_LOOP('',(#8800));
#2433=EDGE_LOOP('',(#8801));
#2434=EDGE_LOOP('',(#8802));
#2435=EDGE_LOOP('',(#8803));
#2436=EDGE_LOOP('',(#8804));
#2437=EDGE_LOOP('',(#8805));
#2438=EDGE_LOOP('',(#8806));
#2439=EDGE_LOOP('',(#8807,#8808,#8809,#8810));
#2440=EDGE_LOOP('',(#8811,#8812,#8813,#8814));
#2441=EDGE_LOOP('',(#8815,#8816,#8817,#8818));
#2442=EDGE_LOOP('',(#8819,#8820,#8821,#8822));
#2443=EDGE_LOOP('',(#8823));
#2444=EDGE_LOOP('',(#8824));
#2445=EDGE_LOOP('',(#8825,#8826,#8827,#8828));
#2446=EDGE_LOOP('',(#8829,#8830,#8831,#8832));
#2447=EDGE_LOOP('',(#8833));
#2448=EDGE_LOOP('',(#8834,#8835,#8836,#8837));
#2449=EDGE_LOOP('',(#8838));
#2450=EDGE_LOOP('',(#8839,#8840,#8841,#8842));
#2451=EDGE_LOOP('',(#8843,#8844,#8845,#8846));
#2452=EDGE_LOOP('',(#8847));
#2453=EDGE_LOOP('',(#8848));
#2454=EDGE_LOOP('',(#8849));
#2455=EDGE_LOOP('',(#8850));
#2456=EDGE_LOOP('',(#8851,#8852,#8853,#8854));
#2457=EDGE_LOOP('',(#8855,#8856,#8857,#8858));
#2458=EDGE_LOOP('',(#8859));
#2459=EDGE_LOOP('',(#8860));
#2460=EDGE_LOOP('',(#8861));
#2461=EDGE_LOOP('',(#8862));
#2462=EDGE_LOOP('',(#8863,#8864,#8865,#8866));
#2463=EDGE_LOOP('',(#8867,#8868,#8869,#8870));
#2464=EDGE_LOOP('',(#8871));
#2465=EDGE_LOOP('',(#8872));
#2466=EDGE_LOOP('',(#8873,#8874,#8875,#8876));
#2467=EDGE_LOOP('',(#8877,#8878));
#2468=EDGE_LOOP('',(#8879));
#2469=EDGE_LOOP('',(#8880));
#2470=EDGE_LOOP('',(#8881));
#2471=EDGE_LOOP('',(#8882));
#2472=EDGE_LOOP('',(#8883,#8884,#8885,#8886));
#2473=EDGE_LOOP('',(#8887,#8888,#8889,#8890));
#2474=EDGE_LOOP('',(#8891,#8892,#8893,#8894));
#2475=EDGE_LOOP('',(#8895,#8896,#8897,#8898));
#2476=EDGE_LOOP('',(#8899,#8900,#8901,#8902));
#2477=EDGE_LOOP('',(#8903));
#2478=EDGE_LOOP('',(#8904));
#2479=EDGE_LOOP('',(#8905,#8906,#8907,#8908));
#2480=EDGE_LOOP('',(#8909,#8910));
#2481=EDGE_LOOP('',(#8911));
#2482=EDGE_LOOP('',(#8912));
#2483=EDGE_LOOP('',(#8913));
#2484=EDGE_LOOP('',(#8914));
#2485=EDGE_LOOP('',(#8915,#8916,#8917));
#2486=EDGE_LOOP('',(#8918));
#2487=EDGE_LOOP('',(#8919,#8920,#8921,#8922,#8923,#8924,#8925,#8926));
#2488=EDGE_LOOP('',(#8927,#8928,#8929));
#2489=EDGE_LOOP('',(#8930));
#2490=EDGE_LOOP('',(#8931,#8932,#8933,#8934,#8935,#8936,#8937,#8938));
#2491=EDGE_LOOP('',(#8939,#8940,#8941,#8942,#8943,#8944,#8945,#8946));
#2492=EDGE_LOOP('',(#8947,#8948,#8949,#8950,#8951,#8952,#8953,#8954));
#2493=EDGE_LOOP('',(#8955,#8956,#8957,#8958));
#2494=EDGE_LOOP('',(#8959,#8960,#8961,#8962));
#2495=EDGE_LOOP('',(#8963,#8964,#8965,#8966,#8967,#8968,#8969,#8970));
#2496=EDGE_LOOP('',(#8971,#8972,#8973,#8974,#8975,#8976,#8977,#8978));
#2497=EDGE_LOOP('',(#8979,#8980,#8981,#8982));
#2498=EDGE_LOOP('',(#8983));
#2499=EDGE_LOOP('',(#8984,#8985,#8986,#8987));
#2500=EDGE_LOOP('',(#8988,#8989,#8990,#8991));
#2501=EDGE_LOOP('',(#8992,#8993,#8994,#8995,#8996,#8997,#8998,#8999));
#2502=EDGE_LOOP('',(#9000,#9001,#9002,#9003));
#2503=EDGE_LOOP('',(#9004));
#2504=EDGE_LOOP('',(#9005));
#2505=EDGE_LOOP('',(#9006,#9007,#9008,#9009));
#2506=EDGE_LOOP('',(#9010));
#2507=EDGE_LOOP('',(#9011,#9012,#9013));
#2508=EDGE_LOOP('',(#9014));
#2509=EDGE_LOOP('',(#9015,#9016,#9017,#9018,#9019,#9020,#9021,#9022));
#2510=EDGE_LOOP('',(#9023,#9024,#9025));
#2511=EDGE_LOOP('',(#9026));
#2512=EDGE_LOOP('',(#9027,#9028,#9029,#9030,#9031,#9032,#9033,#9034));
#2513=EDGE_LOOP('',(#9035,#9036,#9037,#9038,#9039,#9040,#9041,#9042));
#2514=EDGE_LOOP('',(#9043,#9044,#9045,#9046,#9047,#9048,#9049,#9050));
#2515=EDGE_LOOP('',(#9051,#9052,#9053,#9054));
#2516=EDGE_LOOP('',(#9055,#9056,#9057,#9058));
#2517=EDGE_LOOP('',(#9059,#9060,#9061,#9062,#9063,#9064,#9065,#9066));
#2518=EDGE_LOOP('',(#9067,#9068,#9069,#9070,#9071,#9072,#9073,#9074));
#2519=EDGE_LOOP('',(#9075,#9076,#9077,#9078));
#2520=EDGE_LOOP('',(#9079));
#2521=EDGE_LOOP('',(#9080,#9081,#9082,#9083));
#2522=EDGE_LOOP('',(#9084,#9085,#9086,#9087));
#2523=EDGE_LOOP('',(#9088,#9089,#9090,#9091,#9092,#9093,#9094,#9095));
#2524=EDGE_LOOP('',(#9096,#9097,#9098,#9099));
#2525=EDGE_LOOP('',(#9100));
#2526=EDGE_LOOP('',(#9101));
#2527=EDGE_LOOP('',(#9102,#9103,#9104,#9105));
#2528=EDGE_LOOP('',(#9106));
#2529=EDGE_LOOP('',(#9107,#9108,#9109,#9110));
#2530=EDGE_LOOP('',(#9111));
#2531=EDGE_LOOP('',(#9112));
#2532=EDGE_LOOP('',(#9113,#9114,#9115,#9116));
#2533=EDGE_LOOP('',(#9117));
#2534=EDGE_LOOP('',(#9118));
#2535=EDGE_LOOP('',(#9119,#9120,#9121,#9122));
#2536=EDGE_LOOP('',(#9123));
#2537=EDGE_LOOP('',(#9124));
#2538=EDGE_LOOP('',(#9125,#9126,#9127,#9128));
#2539=EDGE_LOOP('',(#9129));
#2540=EDGE_LOOP('',(#9130));
#2541=EDGE_LOOP('',(#9131,#9132,#9133,#9134));
#2542=EDGE_LOOP('',(#9135,#9136,#9137,#9138));
#2543=EDGE_LOOP('',(#9139,#9140,#9141,#9142));
#2544=EDGE_LOOP('',(#9143,#9144,#9145,#9146));
#2545=EDGE_LOOP('',(#9147,#9148,#9149,#9150));
#2546=EDGE_LOOP('',(#9151,#9152,#9153,#9154));
#2547=EDGE_LOOP('',(#9155,#9156,#9157,#9158));
#2548=EDGE_LOOP('',(#9159,#9160,#9161,#9162));
#2549=EDGE_LOOP('',(#9163,#9164,#9165,#9166));
#2550=EDGE_LOOP('',(#9167));
#2551=EDGE_LOOP('',(#9168));
#2552=EDGE_LOOP('',(#9169));
#2553=EDGE_LOOP('',(#9170));
#2554=EDGE_LOOP('',(#9171,#9172,#9173,#9174));
#2555=EDGE_LOOP('',(#9175,#9176,#9177,#9178));
#2556=EDGE_LOOP('',(#9179,#9180,#9181,#9182));
#2557=EDGE_LOOP('',(#9183,#9184,#9185,#9186));
#2558=EDGE_LOOP('',(#9187,#9188,#9189,#9190));
#2559=EDGE_LOOP('',(#9191,#9192,#9193,#9194));
#2560=EDGE_LOOP('',(#9195));
#2561=EDGE_LOOP('',(#9196));
#2562=EDGE_LOOP('',(#9197));
#2563=EDGE_LOOP('',(#9198));
#2564=EDGE_LOOP('',(#9199,#9200,#9201,#9202));
#2565=EDGE_LOOP('',(#9203,#9204,#9205,#9206,#9207,#9208,#9209,#9210,#9211,
#9212,#9213,#9214));
#2566=EDGE_LOOP('',(#9215,#9216,#9217,#9218,#9219,#9220,#9221,#9222,#9223,
#9224,#9225,#9226));
#2567=EDGE_LOOP('',(#9227,#9228,#9229,#9230,#9231,#9232));
#2568=EDGE_LOOP('',(#9233,#9234,#9235,#9236,#9237));
#2569=EDGE_LOOP('',(#9238,#9239,#9240,#9241));
#2570=EDGE_LOOP('',(#9242,#9243,#9244,#9245));
#2571=EDGE_LOOP('',(#9246));
#2572=EDGE_LOOP('',(#9247));
#2573=EDGE_LOOP('',(#9248,#9249,#9250,#9251,#9252));
#2574=EDGE_LOOP('',(#9253));
#2575=EDGE_LOOP('',(#9254));
#2576=EDGE_LOOP('',(#9255,#9256,#9257,#9258));
#2577=EDGE_LOOP('',(#9259,#9260,#9261,#9262,#9263,#9264));
#2578=EDGE_LOOP('',(#9265,#9266,#9267,#9268,#9269));
#2579=EDGE_LOOP('',(#9270));
#2580=EDGE_LOOP('',(#9271));
#2581=EDGE_LOOP('',(#9272,#9273,#9274,#9275));
#2582=EDGE_LOOP('',(#9276,#9277,#9278,#9279));
#2583=EDGE_LOOP('',(#9280,#9281,#9282,#9283));
#2584=EDGE_LOOP('',(#9284));
#2585=EDGE_LOOP('',(#9285));
#2586=EDGE_LOOP('',(#9286,#9287,#9288,#9289,#9290));
#2587=EDGE_LOOP('',(#9291,#9292));
#2588=EDGE_LOOP('',(#9293,#9294));
#2589=EDGE_LOOP('',(#9295,#9296));
#2590=EDGE_LOOP('',(#9297,#9298));
#2591=EDGE_LOOP('',(#9299,#9300));
#2592=EDGE_LOOP('',(#9301,#9302));
#2593=EDGE_LOOP('',(#9303,#9304));
#2594=EDGE_LOOP('',(#9305,#9306,#9307,#9308));
#2595=EDGE_LOOP('',(#9309,#9310,#9311,#9312,#9313,#9314,#9315,#9316,#9317,
#9318,#9319,#9320,#9321,#9322,#9323,#9324,#9325,#9326));
#2596=EDGE_LOOP('',(#9327,#9328,#9329,#9330));
#2597=EDGE_LOOP('',(#9331,#9332,#9333,#9334));
#2598=EDGE_LOOP('',(#9335,#9336,#9337,#9338));
#2599=EDGE_LOOP('',(#9339,#9340,#9341,#9342));
#2600=EDGE_LOOP('',(#9343,#9344,#9345,#9346,#9347,#9348));
#2601=EDGE_LOOP('',(#9349,#9350,#9351,#9352));
#2602=EDGE_LOOP('',(#9353,#9354,#9355,#9356));
#2603=EDGE_LOOP('',(#9357,#9358,#9359,#9360));
#2604=EDGE_LOOP('',(#9361,#9362,#9363,#9364));
#2605=EDGE_LOOP('',(#9365,#9366,#9367,#9368));
#2606=EDGE_LOOP('',(#9369,#9370,#9371,#9372,#9373,#9374,#9375,#9376,#9377,
#9378,#9379,#9380,#9381,#9382,#9383,#9384,#9385,#9386));
#2607=EDGE_LOOP('',(#9387,#9388,#9389,#9390));
#2608=EDGE_LOOP('',(#9391,#9392,#9393,#9394));
#2609=EDGE_LOOP('',(#9395));
#2610=EDGE_LOOP('',(#9396));
#2611=EDGE_LOOP('',(#9397,#9398,#9399,#9400));
#2612=EDGE_LOOP('',(#9401));
#2613=EDGE_LOOP('',(#9402));
#2614=EDGE_LOOP('',(#9403,#9404,#9405,#9406));
#2615=EDGE_LOOP('',(#9407));
#2616=EDGE_LOOP('',(#9408));
#2617=EDGE_LOOP('',(#9409,#9410,#9411,#9412));
#2618=EDGE_LOOP('',(#9413));
#2619=EDGE_LOOP('',(#9414));
#2620=EDGE_LOOP('',(#9415,#9416,#9417,#9418));
#2621=EDGE_LOOP('',(#9419));
#2622=EDGE_LOOP('',(#9420));
#2623=EDGE_LOOP('',(#9421,#9422,#9423,#9424));
#2624=EDGE_LOOP('',(#9425,#9426,#9427,#9428,#9429,#9430));
#2625=EDGE_LOOP('',(#9431,#9432,#9433,#9434,#9435));
#2626=EDGE_LOOP('',(#9436,#9437,#9438,#9439));
#2627=EDGE_LOOP('',(#9440,#9441,#9442,#9443));
#2628=EDGE_LOOP('',(#9444));
#2629=EDGE_LOOP('',(#9445));
#2630=EDGE_LOOP('',(#9446,#9447,#9448,#9449,#9450));
#2631=EDGE_LOOP('',(#9451));
#2632=EDGE_LOOP('',(#9452));
#2633=EDGE_LOOP('',(#9453,#9454,#9455,#9456));
#2634=EDGE_LOOP('',(#9457,#9458,#9459,#9460,#9461,#9462));
#2635=EDGE_LOOP('',(#9463,#9464,#9465,#9466,#9467));
#2636=EDGE_LOOP('',(#9468));
#2637=EDGE_LOOP('',(#9469));
#2638=EDGE_LOOP('',(#9470,#9471,#9472,#9473));
#2639=EDGE_LOOP('',(#9474,#9475,#9476,#9477));
#2640=EDGE_LOOP('',(#9478,#9479,#9480,#9481));
#2641=EDGE_LOOP('',(#9482));
#2642=EDGE_LOOP('',(#9483));
#2643=EDGE_LOOP('',(#9484,#9485,#9486,#9487,#9488));
#2644=EDGE_LOOP('',(#9489,#9490));
#2645=EDGE_LOOP('',(#9491,#9492));
#2646=EDGE_LOOP('',(#9493,#9494));
#2647=EDGE_LOOP('',(#9495,#9496));
#2648=EDGE_LOOP('',(#9497,#9498));
#2649=EDGE_LOOP('',(#9499,#9500));
#2650=EDGE_LOOP('',(#9501,#9502));
#2651=EDGE_LOOP('',(#9503,#9504));
#2652=EDGE_LOOP('',(#9505,#9506,#9507,#9508));
#2653=EDGE_LOOP('',(#9509,#9510,#9511,#9512,#9513,#9514,#9515,#9516,#9517,
#9518,#9519,#9520,#9521,#9522,#9523,#9524,#9525,#9526,#9527,#9528));
#2654=EDGE_LOOP('',(#9529,#9530,#9531,#9532));
#2655=EDGE_LOOP('',(#9533,#9534,#9535,#9536));
#2656=EDGE_LOOP('',(#9537,#9538,#9539,#9540));
#2657=EDGE_LOOP('',(#9541,#9542,#9543,#9544));
#2658=EDGE_LOOP('',(#9545,#9546,#9547,#9548));
#2659=EDGE_LOOP('',(#9549,#9550,#9551,#9552,#9553,#9554));
#2660=EDGE_LOOP('',(#9555,#9556,#9557,#9558));
#2661=EDGE_LOOP('',(#9559,#9560,#9561,#9562));
#2662=EDGE_LOOP('',(#9563,#9564,#9565,#9566));
#2663=EDGE_LOOP('',(#9567,#9568,#9569,#9570));
#2664=EDGE_LOOP('',(#9571,#9572,#9573,#9574));
#2665=EDGE_LOOP('',(#9575,#9576,#9577,#9578));
#2666=EDGE_LOOP('',(#9579,#9580,#9581,#9582,#9583,#9584,#9585,#9586,#9587,
#9588,#9589,#9590,#9591,#9592,#9593,#9594,#9595,#9596,#9597,#9598));
#2667=EDGE_LOOP('',(#9599,#9600,#9601,#9602));
#2668=EDGE_LOOP('',(#9603,#9604,#9605,#9606));
#2669=EDGE_LOOP('',(#9607));
#2670=EDGE_LOOP('',(#9608));
#2671=EDGE_LOOP('',(#9609,#9610,#9611,#9612));
#2672=EDGE_LOOP('',(#9613));
#2673=EDGE_LOOP('',(#9614));
#2674=EDGE_LOOP('',(#9615,#9616,#9617,#9618));
#2675=EDGE_LOOP('',(#9619));
#2676=EDGE_LOOP('',(#9620));
#2677=EDGE_LOOP('',(#9621,#9622,#9623,#9624));
#2678=EDGE_LOOP('',(#9625));
#2679=EDGE_LOOP('',(#9626));
#2680=EDGE_LOOP('',(#9627,#9628,#9629,#9630));
#2681=EDGE_LOOP('',(#9631));
#2682=EDGE_LOOP('',(#9632));
#2683=EDGE_LOOP('',(#9633,#9634,#9635,#9636));
#2684=EDGE_LOOP('',(#9637,#9638,#9639,#9640));
#2685=EDGE_LOOP('',(#9641,#9642,#9643,#9644));
#2686=EDGE_LOOP('',(#9645,#9646,#9647,#9648));
#2687=EDGE_LOOP('',(#9649,#9650,#9651,#9652));
#2688=EDGE_LOOP('',(#9653,#9654,#9655,#9656));
#2689=EDGE_LOOP('',(#9657,#9658,#9659,#9660));
#2690=EDGE_LOOP('',(#9661,#9662,#9663,#9664));
#2691=EDGE_LOOP('',(#9665,#9666,#9667,#9668));
#2692=EDGE_LOOP('',(#9669,#9670,#9671,#9672));
#2693=EDGE_LOOP('',(#9673,#9674,#9675,#9676));
#2694=EDGE_LOOP('',(#9677,#9678,#9679,#9680));
#2695=EDGE_LOOP('',(#9681,#9682,#9683,#9684));
#2696=EDGE_LOOP('',(#9685,#9686,#9687,#9688));
#2697=EDGE_LOOP('',(#9689,#9690,#9691,#9692));
#2698=EDGE_LOOP('',(#9693,#9694,#9695,#9696));
#2699=EDGE_LOOP('',(#9697,#9698,#9699,#9700));
#2700=EDGE_LOOP('',(#9701,#9702,#9703,#9704));
#2701=EDGE_LOOP('',(#9705,#9706,#9707,#9708));
#2702=EDGE_LOOP('',(#9709,#9710,#9711,#9712));
#2703=EDGE_LOOP('',(#9713,#9714,#9715,#9716));
#2704=EDGE_LOOP('',(#9717,#9718,#9719,#9720));
#2705=EDGE_LOOP('',(#9721,#9722,#9723,#9724));
#2706=EDGE_LOOP('',(#9725,#9726,#9727,#9728));
#2707=EDGE_LOOP('',(#9729,#9730,#9731,#9732));
#2708=EDGE_LOOP('',(#9733,#9734,#9735,#9736));
#2709=EDGE_LOOP('',(#9737,#9738,#9739,#9740));
#2710=EDGE_LOOP('',(#9741,#9742,#9743,#9744));
#2711=EDGE_LOOP('',(#9745,#9746,#9747,#9748));
#2712=EDGE_LOOP('',(#9749,#9750,#9751,#9752));
#2713=EDGE_LOOP('',(#9753,#9754,#9755,#9756));
#2714=EDGE_LOOP('',(#9757,#9758,#9759,#9760));
#2715=EDGE_LOOP('',(#9761,#9762,#9763,#9764));
#2716=EDGE_LOOP('',(#9765,#9766,#9767,#9768));
#2717=EDGE_LOOP('',(#9769,#9770,#9771,#9772));
#2718=EDGE_LOOP('',(#9773,#9774,#9775,#9776));
#2719=EDGE_LOOP('',(#9777,#9778,#9779,#9780));
#2720=EDGE_LOOP('',(#9781,#9782,#9783,#9784));
#2721=EDGE_LOOP('',(#9785,#9786,#9787,#9788));
#2722=EDGE_LOOP('',(#9789,#9790,#9791,#9792));
#2723=EDGE_LOOP('',(#9793,#9794,#9795,#9796));
#2724=EDGE_LOOP('',(#9797,#9798,#9799,#9800));
#2725=EDGE_LOOP('',(#9801,#9802,#9803,#9804));
#2726=EDGE_LOOP('',(#9805,#9806,#9807,#9808));
#2727=EDGE_LOOP('',(#9809,#9810,#9811,#9812));
#2728=EDGE_LOOP('',(#9813,#9814,#9815,#9816));
#2729=EDGE_LOOP('',(#9817,#9818,#9819,#9820,#9821,#9822,#9823,#9824,#9825,
#9826,#9827,#9828,#9829,#9830,#9831,#9832,#9833,#9834,#9835,#9836,#9837,
#9838,#9839,#9840,#9841,#9842,#9843,#9844,#9845,#9846,#9847,#9848,#9849,
#9850,#9851,#9852,#9853,#9854,#9855,#9856,#9857,#9858,#9859,#9860));
#2730=EDGE_LOOP('',(#9861));
#2731=EDGE_LOOP('',(#9862,#9863,#9864,#9865,#9866,#9867,#9868,#9869,#9870,
#9871,#9872,#9873,#9874,#9875,#9876,#9877,#9878,#9879,#9880,#9881,#9882,
#9883,#9884,#9885,#9886,#9887,#9888,#9889,#9890,#9891,#9892,#9893,#9894,
#9895,#9896,#9897,#9898,#9899,#9900,#9901,#9902,#9903,#9904,#9905));
#2732=EDGE_LOOP('',(#9906));
#2733=EDGE_LOOP('',(#9907,#9908,#9909,#9910,#9911,#9912));
#2734=EDGE_LOOP('',(#9913,#9914,#9915,#9916,#9917,#9918,#9919,#9920));
#2735=EDGE_LOOP('',(#9921,#9922,#9923,#9924,#9925));
#2736=EDGE_LOOP('',(#9926,#9927,#9928,#9929));
#2737=EDGE_LOOP('',(#9930,#9931,#9932,#9933,#9934,#9935));
#2738=EDGE_LOOP('',(#9936,#9937,#9938,#9939,#9940,#9941));
#2739=EDGE_LOOP('',(#9942,#9943,#9944,#9945));
#2740=EDGE_LOOP('',(#9946,#9947,#9948,#9949));
#2741=EDGE_LOOP('',(#9950,#9951,#9952,#9953,#9954,#9955));
#2742=EDGE_LOOP('',(#9956,#9957,#9958,#9959));
#2743=EDGE_LOOP('',(#9960));
#2744=EDGE_LOOP('',(#9961,#9962,#9963,#9964));
#2745=EDGE_LOOP('',(#9965,#9966,#9967,#9968));
#2746=EDGE_LOOP('',(#9969));
#2747=EDGE_LOOP('',(#9970));
#2748=EDGE_LOOP('',(#9971,#9972,#9973,#9974));
#2749=EDGE_LOOP('',(#9975));
#2750=EDGE_LOOP('',(#9976));
#2751=EDGE_LOOP('',(#9977,#9978,#9979,#9980));
#2752=EDGE_LOOP('',(#9981,#9982,#9983,#9984));
#2753=EDGE_LOOP('',(#9985,#9986,#9987,#9988));
#2754=EDGE_LOOP('',(#9989,#9990,#9991,#9992));
#2755=EDGE_LOOP('',(#9993,#9994,#9995,#9996));
#2756=EDGE_LOOP('',(#9997,#9998,#9999,#10000));
#2757=EDGE_LOOP('',(#10001,#10002,#10003,#10004,#10005,#10006));
#2758=EDGE_LOOP('',(#10007,#10008,#10009,#10010,#10011,#10012));
#2759=EDGE_LOOP('',(#10013));
#2760=EDGE_LOOP('',(#10014));
#2761=EDGE_LOOP('',(#10015,#10016,#10017,#10018));
#2762=EDGE_LOOP('',(#10019,#10020,#10021,#10022));
#2763=EDGE_LOOP('',(#10023,#10024,#10025,#10026));
#2764=EDGE_LOOP('',(#10027));
#2765=EDGE_LOOP('',(#10028));
#2766=EDGE_LOOP('',(#10029,#10030,#10031,#10032));
#2767=EDGE_LOOP('',(#10033,#10034,#10035,#10036));
#2768=EDGE_LOOP('',(#10037,#10038,#10039,#10040));
#2769=EDGE_LOOP('',(#10041,#10042,#10043,#10044));
#2770=EDGE_LOOP('',(#10045,#10046,#10047,#10048));
#2771=EDGE_LOOP('',(#10049,#10050,#10051,#10052));
#2772=EDGE_LOOP('',(#10053,#10054,#10055,#10056));
#2773=EDGE_LOOP('',(#10057,#10058,#10059,#10060));
#2774=EDGE_LOOP('',(#10061,#10062,#10063,#10064));
#2775=EDGE_LOOP('',(#10065,#10066,#10067,#10068));
#2776=EDGE_LOOP('',(#10069,#10070,#10071,#10072));
#2777=EDGE_LOOP('',(#10073));
#2778=EDGE_LOOP('',(#10074));
#2779=EDGE_LOOP('',(#10075));
#2780=EDGE_LOOP('',(#10076));
#2781=EDGE_LOOP('',(#10077,#10078,#10079,#10080));
#2782=EDGE_LOOP('',(#10081));
#2783=EDGE_LOOP('',(#10082));
#2784=EDGE_LOOP('',(#10083));
#2785=EDGE_LOOP('',(#10084));
#2786=EDGE_LOOP('',(#10085,#10086,#10087,#10088));
#2787=EDGE_LOOP('',(#10089,#10090,#10091,#10092));
#2788=EDGE_LOOP('',(#10093,#10094,#10095,#10096));
#2789=EDGE_LOOP('',(#10097,#10098,#10099,#10100));
#2790=EDGE_LOOP('',(#10101,#10102,#10103,#10104));
#2791=EDGE_LOOP('',(#10105,#10106,#10107,#10108));
#2792=EDGE_LOOP('',(#10109,#10110,#10111,#10112));
#2793=EDGE_LOOP('',(#10113,#10114,#10115,#10116));
#2794=EDGE_LOOP('',(#10117,#10118,#10119,#10120));
#2795=EDGE_LOOP('',(#10121,#10122,#10123,#10124));
#2796=EDGE_LOOP('',(#10125,#10126,#10127,#10128));
#2797=EDGE_LOOP('',(#10129,#10130,#10131,#10132));
#2798=EDGE_LOOP('',(#10133,#10134,#10135,#10136));
#2799=EDGE_LOOP('',(#10137));
#2800=EDGE_LOOP('',(#10138));
#2801=EDGE_LOOP('',(#10139));
#2802=EDGE_LOOP('',(#10140));
#2803=EDGE_LOOP('',(#10141));
#2804=EDGE_LOOP('',(#10142));
#2805=EDGE_LOOP('',(#10143));
#2806=EDGE_LOOP('',(#10144));
#2807=EDGE_LOOP('',(#10145,#10146,#10147,#10148));
#2808=EDGE_LOOP('',(#10149));
#2809=EDGE_LOOP('',(#10150));
#2810=EDGE_LOOP('',(#10151));
#2811=EDGE_LOOP('',(#10152));
#2812=EDGE_LOOP('',(#10153));
#2813=EDGE_LOOP('',(#10154));
#2814=EDGE_LOOP('',(#10155));
#2815=EDGE_LOOP('',(#10156));
#2816=EDGE_LOOP('',(#10157,#10158,#10159,#10160));
#2817=EDGE_LOOP('',(#10161));
#2818=EDGE_LOOP('',(#10162,#10163,#10164,#10165));
#2819=EDGE_LOOP('',(#10166));
#2820=EDGE_LOOP('',(#10167,#10168,#10169,#10170));
#2821=EDGE_LOOP('',(#10171));
#2822=EDGE_LOOP('',(#10172,#10173,#10174,#10175));
#2823=EDGE_LOOP('',(#10176));
#2824=EDGE_LOOP('',(#10177,#10178,#10179,#10180));
#2825=EDGE_LOOP('',(#10181));
#2826=EDGE_LOOP('',(#10182,#10183,#10184,#10185));
#2827=EDGE_LOOP('',(#10186));
#2828=EDGE_LOOP('',(#10187,#10188,#10189,#10190));
#2829=EDGE_LOOP('',(#10191));
#2830=EDGE_LOOP('',(#10192,#10193,#10194,#10195));
#2831=EDGE_LOOP('',(#10196,#10197,#10198,#10199));
#2832=EDGE_LOOP('',(#10200,#10201,#10202,#10203));
#2833=EDGE_LOOP('',(#10204));
#2834=EDGE_LOOP('',(#10205));
#2835=EDGE_LOOP('',(#10206));
#2836=EDGE_LOOP('',(#10207));
#2837=EDGE_LOOP('',(#10208,#10209,#10210,#10211));
#2838=EDGE_LOOP('',(#10212,#10213,#10214,#10215));
#2839=EDGE_LOOP('',(#10216));
#2840=EDGE_LOOP('',(#10217,#10218,#10219,#10220));
#2841=EDGE_LOOP('',(#10221));
#2842=EDGE_LOOP('',(#10222));
#2843=EDGE_LOOP('',(#10223));
#2844=EDGE_LOOP('',(#10224));
#2845=EDGE_LOOP('',(#10225,#10226,#10227,#10228));
#2846=EDGE_LOOP('',(#10229,#10230));
#2847=EDGE_LOOP('',(#10231,#10232,#10233,#10234,#10235,#10236,#10237,#10238));
#2848=EDGE_LOOP('',(#10239,#10240));
#2849=EDGE_LOOP('',(#10241,#10242,#10243,#10244,#10245,#10246,#10247,#10248));
#2850=EDGE_LOOP('',(#10249,#10250));
#2851=EDGE_LOOP('',(#10251,#10252,#10253,#10254,#10255,#10256,#10257,#10258));
#2852=EDGE_LOOP('',(#10259,#10260));
#2853=EDGE_LOOP('',(#10261,#10262,#10263,#10264,#10265,#10266,#10267,#10268));
#2854=EDGE_LOOP('',(#10269,#10270,#10271,#10272,#10273,#10274,#10275,#10276,
#10277,#10278,#10279,#10280));
#2855=EDGE_LOOP('',(#10281,#10282,#10283,#10284,#10285,#10286,#10287,#10288,
#10289,#10290,#10291,#10292));
#2856=EDGE_LOOP('',(#10293,#10294,#10295,#10296,#10297,#10298,#10299,#10300,
#10301,#10302,#10303,#10304));
#2857=EDGE_LOOP('',(#10305,#10306,#10307,#10308,#10309,#10310,#10311,#10312,
#10313,#10314));
#2858=EDGE_LOOP('',(#10315,#10316,#10317,#10318));
#2859=EDGE_LOOP('',(#10319,#10320,#10321,#10322));
#2860=EDGE_LOOP('',(#10323));
#2861=EDGE_LOOP('',(#10324));
#2862=EDGE_LOOP('',(#10325));
#2863=EDGE_LOOP('',(#10326));
#2864=EDGE_LOOP('',(#10327,#10328,#10329,#10330));
#2865=EDGE_LOOP('',(#10331,#10332,#10333,#10334,#10335,#10336,#10337,#10338,
#10339,#10340));
#2866=EDGE_LOOP('',(#10341,#10342,#10343,#10344));
#2867=EDGE_LOOP('',(#10345,#10346,#10347,#10348));
#2868=EDGE_LOOP('',(#10349,#10350,#10351,#10352));
#2869=EDGE_LOOP('',(#10353,#10354,#10355,#10356));
#2870=EDGE_LOOP('',(#10357,#10358,#10359,#10360));
#2871=EDGE_LOOP('',(#10361,#10362,#10363,#10364,#10365,#10366,#10367,#10368,
#10369,#10370,#10371,#10372));
#2872=EDGE_LOOP('',(#10373,#10374,#10375,#10376));
#2873=EDGE_LOOP('',(#10377,#10378,#10379,#10380));
#2874=EDGE_LOOP('',(#10381,#10382,#10383,#10384));
#2875=EDGE_LOOP('',(#10385,#10386,#10387,#10388));
#2876=EDGE_LOOP('',(#10389,#10390,#10391,#10392));
#2877=EDGE_LOOP('',(#10393,#10394,#10395,#10396));
#2878=EDGE_LOOP('',(#10397,#10398,#10399,#10400));
#2879=EDGE_LOOP('',(#10401,#10402,#10403,#10404));
#2880=EDGE_LOOP('',(#10405,#10406,#10407,#10408,#10409,#10410,#10411,#10412));
#2881=EDGE_LOOP('',(#10413,#10414,#10415,#10416,#10417,#10418,#10419,#10420));
#2882=EDGE_LOOP('',(#10421,#10422,#10423,#10424));
#2883=EDGE_LOOP('',(#10425,#10426,#10427,#10428));
#2884=EDGE_LOOP('',(#10429,#10430,#10431,#10432));
#2885=EDGE_LOOP('',(#10433,#10434,#10435,#10436));
#2886=EDGE_LOOP('',(#10437,#10438,#10439,#10440));
#2887=EDGE_LOOP('',(#10441,#10442,#10443,#10444));
#2888=EDGE_LOOP('',(#10445,#10446,#10447,#10448));
#2889=EDGE_LOOP('',(#10449,#10450,#10451,#10452));
#2890=EDGE_LOOP('',(#10453,#10454,#10455,#10456,#10457,#10458,#10459,#10460));
#2891=EDGE_LOOP('',(#10461,#10462,#10463,#10464,#10465,#10466,#10467,#10468));
#2892=EDGE_LOOP('',(#10469,#10470,#10471,#10472));
#2893=EDGE_LOOP('',(#10473,#10474,#10475,#10476));
#2894=EDGE_LOOP('',(#10477));
#2895=EDGE_LOOP('',(#10478));
#2896=EDGE_LOOP('',(#10479,#10480,#10481,#10482));
#2897=EDGE_LOOP('',(#10483));
#2898=EDGE_LOOP('',(#10484));
#2899=EDGE_LOOP('',(#10485,#10486,#10487,#10488));
#2900=EDGE_LOOP('',(#10489,#10490,#10491,#10492));
#2901=EDGE_LOOP('',(#10493,#10494,#10495,#10496));
#2902=EDGE_LOOP('',(#10497,#10498,#10499,#10500));
#2903=EDGE_LOOP('',(#10501,#10502,#10503,#10504));
#2904=EDGE_LOOP('',(#10505,#10506,#10507,#10508));
#2905=EDGE_LOOP('',(#10509,#10510,#10511,#10512,#10513,#10514));
#2906=EDGE_LOOP('',(#10515,#10516,#10517,#10518,#10519,#10520));
#2907=EDGE_LOOP('',(#10521));
#2908=EDGE_LOOP('',(#10522));
#2909=EDGE_LOOP('',(#10523,#10524,#10525,#10526));
#2910=EDGE_LOOP('',(#10527));
#2911=EDGE_LOOP('',(#10528));
#2912=EDGE_LOOP('',(#10529,#10530,#10531,#10532));
#2913=EDGE_LOOP('',(#10533,#10534,#10535,#10536));
#2914=EDGE_LOOP('',(#10537,#10538,#10539,#10540));
#2915=EDGE_LOOP('',(#10541));
#2916=EDGE_LOOP('',(#10542));
#2917=EDGE_LOOP('',(#10543,#10544,#10545,#10546));
#2918=EDGE_LOOP('',(#10547,#10548,#10549,#10550));
#2919=EDGE_LOOP('',(#10551,#10552,#10553,#10554));
#2920=EDGE_LOOP('',(#10555,#10556,#10557,#10558));
#2921=EDGE_LOOP('',(#10559,#10560,#10561,#10562));
#2922=EDGE_LOOP('',(#10563,#10564,#10565,#10566));
#2923=EDGE_LOOP('',(#10567,#10568,#10569,#10570));
#2924=EDGE_LOOP('',(#10571,#10572,#10573,#10574));
#2925=EDGE_LOOP('',(#10575,#10576,#10577,#10578));
#2926=EDGE_LOOP('',(#10579,#10580,#10581,#10582));
#2927=EDGE_LOOP('',(#10583,#10584,#10585));
#2928=EDGE_LOOP('',(#10586,#10587,#10588,#10589));
#2929=EDGE_LOOP('',(#10590,#10591,#10592,#10593));
#2930=EDGE_LOOP('',(#10594,#10595,#10596,#10597));
#2931=EDGE_LOOP('',(#10598,#10599,#10600,#10601));
#2932=EDGE_LOOP('',(#10602,#10603,#10604,#10605));
#2933=EDGE_LOOP('',(#10606,#10607,#10608,#10609));
#2934=EDGE_LOOP('',(#10610,#10611,#10612,#10613));
#2935=EDGE_LOOP('',(#10614,#10615,#10616,#10617));
#2936=EDGE_LOOP('',(#10618,#10619,#10620,#10621));
#2937=EDGE_LOOP('',(#10622,#10623,#10624,#10625));
#2938=EDGE_LOOP('',(#10626,#10627,#10628,#10629,#10630,#10631,#10632,#10633,
#10634,#10635,#10636,#10637,#10638,#10639,#10640,#10641,#10642,#10643,#10644,
#10645,#10646,#10647));
#2939=EDGE_LOOP('',(#10648,#10649,#10650,#10651,#10652,#10653,#10654,#10655,
#10656,#10657,#10658,#10659,#10660,#10661,#10662,#10663,#10664,#10665,#10666,
#10667,#10668));
#2940=EDGE_LOOP('',(#10669,#10670));
#2941=EDGE_LOOP('',(#10671,#10672,#10673,#10674,#10675));
#2942=EDGE_LOOP('',(#10676));
#2943=EDGE_LOOP('',(#10677));
#2944=EDGE_LOOP('',(#10678));
#2945=EDGE_LOOP('',(#10679,#10680,#10681,#10682));
#2946=EDGE_LOOP('',(#10683,#10684,#10685,#10686));
#2947=EDGE_LOOP('',(#10687,#10688,#10689,#10690));
#2948=EDGE_LOOP('',(#10691,#10692,#10693,#10694));
#2949=EDGE_LOOP('',(#10695,#10696));
#2950=EDGE_LOOP('',(#10697));
#2951=EDGE_LOOP('',(#10698));
#2952=EDGE_LOOP('',(#10699));
#2953=EDGE_LOOP('',(#10700));
#2954=EDGE_LOOP('',(#10701,#10702,#10703,#10704));
#2955=EDGE_LOOP('',(#10705,#10706,#10707,#10708,#10709));
#2956=EDGE_LOOP('',(#10710,#10711,#10712,#10713));
#2957=EDGE_LOOP('',(#10714));
#2958=EDGE_LOOP('',(#10715,#10716,#10717,#10718));
#2959=EDGE_LOOP('',(#10719));
#2960=EDGE_LOOP('',(#10720,#10721,#10722,#10723));
#2961=EDGE_LOOP('',(#10724,#10725,#10726,#10727));
#2962=EDGE_LOOP('',(#10728,#10729,#10730,#10731));
#2963=EDGE_LOOP('',(#10732));
#2964=EDGE_LOOP('',(#10733));
#2965=EDGE_LOOP('',(#10734,#10735,#10736,#10737));
#2966=EDGE_LOOP('',(#10738,#10739,#10740,#10741));
#2967=EDGE_LOOP('',(#10742,#10743,#10744,#10745));
#2968=EDGE_LOOP('',(#10746));
#2969=EDGE_LOOP('',(#10747,#10748,#10749,#10750));
#2970=EDGE_LOOP('',(#10751,#10752,#10753,#10754));
#2971=EDGE_LOOP('',(#10755,#10756,#10757,#10758));
#2972=EDGE_LOOP('',(#10759,#10760,#10761,#10762));
#2973=EDGE_LOOP('',(#10763,#10764,#10765,#10766));
#2974=EDGE_LOOP('',(#10767,#10768,#10769,#10770));
#2975=EDGE_LOOP('',(#10771,#10772,#10773,#10774,#10775,#10776));
#2976=EDGE_LOOP('',(#10777,#10778,#10779,#10780,#10781,#10782));
#2977=EDGE_LOOP('',(#10783));
#2978=EDGE_LOOP('',(#10784,#10785,#10786,#10787));
#2979=EDGE_LOOP('',(#10788,#10789,#10790,#10791));
#2980=EDGE_LOOP('',(#10792,#10793,#10794,#10795));
#2981=EDGE_LOOP('',(#10796));
#2982=EDGE_LOOP('',(#10797));
#2983=EDGE_LOOP('',(#10798,#10799,#10800,#10801));
#2984=EDGE_LOOP('',(#10802,#10803,#10804,#10805));
#2985=EDGE_LOOP('',(#10806,#10807,#10808,#10809));
#2986=EDGE_LOOP('',(#10810));
#2987=EDGE_LOOP('',(#10811,#10812,#10813,#10814));
#2988=EDGE_LOOP('',(#10815,#10816,#10817,#10818));
#2989=EDGE_LOOP('',(#10819,#10820,#10821,#10822));
#2990=EDGE_LOOP('',(#10823,#10824,#10825,#10826));
#2991=EDGE_LOOP('',(#10827,#10828,#10829,#10830));
#2992=EDGE_LOOP('',(#10831,#10832,#10833,#10834));
#2993=EDGE_LOOP('',(#10835,#10836,#10837,#10838,#10839,#10840));
#2994=EDGE_LOOP('',(#10841,#10842,#10843,#10844,#10845,#10846));
#2995=EDGE_LOOP('',(#10847,#10848,#10849,#10850));
#2996=EDGE_LOOP('',(#10851,#10852,#10853,#10854));
#2997=EDGE_LOOP('',(#10855,#10856,#10857,#10858));
#2998=EDGE_LOOP('',(#10859,#10860,#10861,#10862));
#2999=EDGE_LOOP('',(#10863,#10864,#10865,#10866));
#3000=EDGE_LOOP('',(#10867,#10868,#10869,#10870));
#3001=EDGE_LOOP('',(#10871,#10872,#10873,#10874));
#3002=EDGE_LOOP('',(#10875,#10876,#10877,#10878));
#3003=EDGE_LOOP('',(#10879,#10880,#10881,#10882));
#3004=EDGE_LOOP('',(#10883,#10884,#10885,#10886));
#3005=EDGE_LOOP('',(#10887,#10888,#10889,#10890));
#3006=EDGE_LOOP('',(#10891,#10892,#10893,#10894));
#3007=EDGE_LOOP('',(#10895,#10896,#10897,#10898));
#3008=EDGE_LOOP('',(#10899,#10900,#10901,#10902));
#3009=EDGE_LOOP('',(#10903,#10904,#10905,#10906));
#3010=EDGE_LOOP('',(#10907,#10908,#10909,#10910));
#3011=EDGE_LOOP('',(#10911,#10912,#10913,#10914));
#3012=EDGE_LOOP('',(#10915,#10916,#10917,#10918));
#3013=EDGE_LOOP('',(#10919,#10920,#10921,#10922));
#3014=EDGE_LOOP('',(#10923,#10924,#10925,#10926));
#3015=EDGE_LOOP('',(#10927,#10928,#10929,#10930));
#3016=EDGE_LOOP('',(#10931,#10932,#10933,#10934));
#3017=EDGE_LOOP('',(#10935,#10936,#10937,#10938));
#3018=EDGE_LOOP('',(#10939,#10940,#10941,#10942));
#3019=EDGE_LOOP('',(#10943,#10944,#10945,#10946));
#3020=EDGE_LOOP('',(#10947,#10948,#10949,#10950));
#3021=EDGE_LOOP('',(#10951,#10952,#10953,#10954));
#3022=EDGE_LOOP('',(#10955,#10956,#10957,#10958));
#3023=EDGE_LOOP('',(#10959,#10960,#10961,#10962));
#3024=EDGE_LOOP('',(#10963,#10964,#10965,#10966));
#3025=EDGE_LOOP('',(#10967,#10968,#10969,#10970));
#3026=EDGE_LOOP('',(#10971,#10972,#10973,#10974));
#3027=EDGE_LOOP('',(#10975,#10976,#10977,#10978));
#3028=EDGE_LOOP('',(#10979,#10980,#10981,#10982));
#3029=EDGE_LOOP('',(#10983,#10984,#10985,#10986));
#3030=EDGE_LOOP('',(#10987,#10988,#10989,#10990));
#3031=EDGE_LOOP('',(#10991,#10992,#10993,#10994));
#3032=EDGE_LOOP('',(#10995,#10996,#10997,#10998));
#3033=EDGE_LOOP('',(#10999,#11000,#11001,#11002));
#3034=EDGE_LOOP('',(#11003,#11004,#11005,#11006));
#3035=EDGE_LOOP('',(#11007,#11008,#11009,#11010));
#3036=EDGE_LOOP('',(#11011,#11012,#11013,#11014));
#3037=EDGE_LOOP('',(#11015,#11016,#11017,#11018));
#3038=EDGE_LOOP('',(#11019,#11020,#11021,#11022));
#3039=EDGE_LOOP('',(#11023,#11024,#11025,#11026));
#3040=EDGE_LOOP('',(#11027,#11028,#11029,#11030));
#3041=EDGE_LOOP('',(#11031,#11032,#11033,#11034));
#3042=EDGE_LOOP('',(#11035,#11036,#11037,#11038));
#3043=EDGE_LOOP('',(#11039,#11040,#11041,#11042));
#3044=EDGE_LOOP('',(#11043,#11044,#11045,#11046));
#3045=EDGE_LOOP('',(#11047,#11048,#11049,#11050));
#3046=EDGE_LOOP('',(#11051,#11052,#11053,#11054));
#3047=EDGE_LOOP('',(#11055,#11056,#11057,#11058));
#3048=EDGE_LOOP('',(#11059,#11060,#11061,#11062));
#3049=EDGE_LOOP('',(#11063,#11064,#11065,#11066));
#3050=EDGE_LOOP('',(#11067,#11068,#11069,#11070));
#3051=EDGE_LOOP('',(#11071,#11072,#11073,#11074));
#3052=EDGE_LOOP('',(#11075,#11076,#11077,#11078));
#3053=EDGE_LOOP('',(#11079,#11080,#11081,#11082));
#3054=EDGE_LOOP('',(#11083,#11084,#11085,#11086));
#3055=EDGE_LOOP('',(#11087,#11088,#11089,#11090));
#3056=EDGE_LOOP('',(#11091,#11092,#11093,#11094));
#3057=EDGE_LOOP('',(#11095,#11096,#11097,#11098));
#3058=EDGE_LOOP('',(#11099,#11100,#11101));
#3059=EDGE_LOOP('',(#11102,#11103,#11104,#11105,#11106));
#3060=EDGE_LOOP('',(#11107,#11108,#11109,#11110));
#3061=EDGE_LOOP('',(#11111,#11112,#11113,#11114));
#3062=EDGE_LOOP('',(#11115,#11116,#11117,#11118));
#3063=EDGE_LOOP('',(#11119,#11120,#11121,#11122));
#3064=EDGE_LOOP('',(#11123,#11124,#11125,#11126));
#3065=EDGE_LOOP('',(#11127,#11128,#11129,#11130));
#3066=EDGE_LOOP('',(#11131,#11132,#11133,#11134));
#3067=EDGE_LOOP('',(#11135,#11136,#11137,#11138));
#3068=EDGE_LOOP('',(#11139,#11140,#11141,#11142));
#3069=EDGE_LOOP('',(#11143,#11144,#11145,#11146));
#3070=EDGE_LOOP('',(#11147,#11148,#11149,#11150));
#3071=EDGE_LOOP('',(#11151,#11152,#11153,#11154));
#3072=EDGE_LOOP('',(#11155,#11156,#11157,#11158));
#3073=EDGE_LOOP('',(#11159,#11160,#11161,#11162));
#3074=EDGE_LOOP('',(#11163,#11164,#11165,#11166));
#3075=EDGE_LOOP('',(#11167,#11168,#11169,#11170));
#3076=EDGE_LOOP('',(#11171,#11172,#11173,#11174));
#3077=EDGE_LOOP('',(#11175,#11176,#11177,#11178));
#3078=EDGE_LOOP('',(#11179,#11180,#11181,#11182));
#3079=EDGE_LOOP('',(#11183,#11184,#11185,#11186));
#3080=EDGE_LOOP('',(#11187,#11188,#11189,#11190));
#3081=EDGE_LOOP('',(#11191,#11192,#11193,#11194));
#3082=EDGE_LOOP('',(#11195,#11196,#11197,#11198));
#3083=EDGE_LOOP('',(#11199,#11200,#11201,#11202));
#3084=EDGE_LOOP('',(#11203,#11204,#11205,#11206));
#3085=EDGE_LOOP('',(#11207,#11208,#11209,#11210));
#3086=EDGE_LOOP('',(#11211,#11212,#11213,#11214));
#3087=EDGE_LOOP('',(#11215,#11216,#11217,#11218));
#3088=EDGE_LOOP('',(#11219,#11220,#11221,#11222));
#3089=EDGE_LOOP('',(#11223,#11224,#11225,#11226));
#3090=EDGE_LOOP('',(#11227,#11228,#11229,#11230));
#3091=EDGE_LOOP('',(#11231,#11232,#11233,#11234));
#3092=EDGE_LOOP('',(#11235,#11236,#11237,#11238));
#3093=EDGE_LOOP('',(#11239,#11240,#11241,#11242));
#3094=EDGE_LOOP('',(#11243,#11244,#11245,#11246));
#3095=EDGE_LOOP('',(#11247,#11248,#11249,#11250));
#3096=EDGE_LOOP('',(#11251,#11252,#11253,#11254));
#3097=EDGE_LOOP('',(#11255,#11256,#11257,#11258));
#3098=EDGE_LOOP('',(#11259,#11260,#11261,#11262));
#3099=EDGE_LOOP('',(#11263,#11264,#11265,#11266));
#3100=EDGE_LOOP('',(#11267,#11268,#11269,#11270));
#3101=EDGE_LOOP('',(#11271,#11272,#11273,#11274));
#3102=EDGE_LOOP('',(#11275,#11276,#11277,#11278));
#3103=EDGE_LOOP('',(#11279,#11280,#11281,#11282));
#3104=EDGE_LOOP('',(#11283,#11284,#11285,#11286));
#3105=EDGE_LOOP('',(#11287,#11288,#11289,#11290));
#3106=EDGE_LOOP('',(#11291,#11292,#11293,#11294));
#3107=EDGE_LOOP('',(#11295,#11296,#11297,#11298));
#3108=EDGE_LOOP('',(#11299,#11300,#11301,#11302));
#3109=EDGE_LOOP('',(#11303,#11304,#11305,#11306));
#3110=EDGE_LOOP('',(#11307,#11308,#11309,#11310));
#3111=EDGE_LOOP('',(#11311,#11312,#11313,#11314));
#3112=EDGE_LOOP('',(#11315,#11316,#11317,#11318));
#3113=EDGE_LOOP('',(#11319,#11320,#11321,#11322));
#3114=EDGE_LOOP('',(#11323,#11324,#11325,#11326));
#3115=EDGE_LOOP('',(#11327,#11328,#11329,#11330));
#3116=EDGE_LOOP('',(#11331,#11332,#11333,#11334));
#3117=EDGE_LOOP('',(#11335,#11336,#11337,#11338));
#3118=EDGE_LOOP('',(#11339,#11340,#11341,#11342));
#3119=EDGE_LOOP('',(#11343,#11344,#11345,#11346));
#3120=EDGE_LOOP('',(#11347,#11348,#11349,#11350));
#3121=EDGE_LOOP('',(#11351));
#3122=EDGE_LOOP('',(#11352,#11353,#11354,#11355));
#3123=EDGE_LOOP('',(#11356,#11357,#11358,#11359));
#3124=EDGE_LOOP('',(#11360));
#3125=EDGE_LOOP('',(#11361,#11362,#11363,#11364,#11365,#11366,#11367,#11368,
#11369,#11370,#11371,#11372,#11373,#11374,#11375,#11376,#11377,#11378,#11379,
#11380,#11381,#11382,#11383,#11384,#11385,#11386,#11387,#11388,#11389,#11390,
#11391,#11392,#11393,#11394,#11395,#11396,#11397,#11398,#11399,#11400,#11401,
#11402,#11403,#11404,#11405,#11406,#11407,#11408,#11409,#11410,#11411,#11412,
#11413,#11414,#11415,#11416,#11417,#11418,#11419,#11420,#11421,#11422,#11423,
#11424,#11425,#11426,#11427,#11428,#11429,#11430,#11431,#11432,#11433,#11434,
#11435,#11436,#11437,#11438,#11439,#11440,#11441,#11442,#11443,#11444,#11445,
#11446,#11447,#11448,#11449,#11450,#11451,#11452,#11453,#11454,#11455,#11456,
#11457,#11458,#11459,#11460,#11461,#11462,#11463,#11464,#11465,#11466,#11467,
#11468,#11469,#11470,#11471,#11472,#11473,#11474,#11475,#11476,#11477,#11478,
#11479,#11480,#11481,#11482,#11483,#11484,#11485,#11486,#11487,#11488,#11489));
#3126=EDGE_LOOP('',(#11490,#11491,#11492,#11493));
#3127=EDGE_LOOP('',(#11494,#11495,#11496,#11497,#11498,#11499,#11500,#11501,
#11502,#11503,#11504,#11505,#11506,#11507,#11508,#11509,#11510,#11511,#11512,
#11513,#11514,#11515,#11516,#11517,#11518,#11519,#11520,#11521,#11522,#11523,
#11524,#11525,#11526,#11527,#11528,#11529,#11530,#11531,#11532,#11533,#11534,
#11535,#11536,#11537,#11538,#11539,#11540,#11541,#11542,#11543,#11544,#11545,
#11546,#11547,#11548,#11549,#11550,#11551,#11552,#11553,#11554,#11555,#11556,
#11557,#11558,#11559,#11560,#11561,#11562,#11563,#11564,#11565,#11566,#11567,
#11568,#11569,#11570,#11571,#11572,#11573,#11574,#11575,#11576,#11577,#11578,
#11579,#11580,#11581,#11582,#11583,#11584,#11585,#11586,#11587,#11588,#11589,
#11590,#11591,#11592,#11593,#11594,#11595,#11596,#11597,#11598,#11599,#11600,
#11601,#11602,#11603,#11604,#11605,#11606,#11607,#11608,#11609,#11610,#11611,
#11612,#11613,#11614,#11615,#11616,#11617,#11618,#11619,#11620,#11621,#11622,
#11623));
#3128=EDGE_LOOP('',(#11624,#11625,#11626,#11627));
#3129=EDGE_LOOP('',(#11628,#11629,#11630,#11631));
#3130=EDGE_LOOP('',(#11632,#11633,#11634,#11635));
#3131=EDGE_LOOP('',(#11636,#11637,#11638,#11639));
#3132=EDGE_LOOP('',(#11640,#11641,#11642,#11643));
#3133=EDGE_LOOP('',(#11644,#11645,#11646,#11647));
#3134=EDGE_LOOP('',(#11648,#11649,#11650,#11651));
#3135=EDGE_LOOP('',(#11652));
#3136=EDGE_LOOP('',(#11653));
#3137=EDGE_LOOP('',(#11654,#11655,#11656,#11657,#11658));
#3138=EDGE_LOOP('',(#11659,#11660,#11661,#11662));
#3139=EDGE_LOOP('',(#11663));
#3140=EDGE_LOOP('',(#11664));
#3141=EDGE_LOOP('',(#11665,#11666,#11667,#11668));
#3142=EDGE_LOOP('',(#11669,#11670,#11671,#11672));
#3143=EDGE_LOOP('',(#11673,#11674,#11675,#11676));
#3144=EDGE_LOOP('',(#11677));
#3145=EDGE_LOOP('',(#11678));
#3146=EDGE_LOOP('',(#11679));
#3147=EDGE_LOOP('',(#11680));
#3148=EDGE_LOOP('',(#11681,#11682));
#3149=EDGE_LOOP('',(#11683,#11684,#11685,#11686,#11687,#11688,#11689,#11690,
#11691));
#3150=EDGE_LOOP('',(#11692,#11693));
#3151=EDGE_LOOP('',(#11694,#11695,#11696,#11697));
#3152=EDGE_LOOP('',(#11698,#11699,#11700,#11701,#11702));
#3153=EDGE_LOOP('',(#11703,#11704,#11705,#11706));
#3154=EDGE_LOOP('',(#11707,#11708));
#3155=EDGE_LOOP('',(#11709));
#3156=EDGE_LOOP('',(#11710));
#3157=EDGE_LOOP('',(#11711));
#3158=EDGE_LOOP('',(#11712));
#3159=EDGE_LOOP('',(#11713,#11714,#11715,#11716));
#3160=EDGE_LOOP('',(#11717,#11718));
#3161=EDGE_LOOP('',(#11719,#11720,#11721,#11722,#11723,#11724,#11725,#11726,
#11727));
#3162=EDGE_LOOP('',(#11728,#11729));
#3163=EDGE_LOOP('',(#11730,#11731,#11732,#11733,#11734,#11735));
#3164=EDGE_LOOP('',(#11736,#11737,#11738,#11739));
#3165=EDGE_LOOP('',(#11740,#11741,#11742,#11743,#11744,#11745));
#3166=EDGE_LOOP('',(#11746));
#3167=EDGE_LOOP('',(#11747));
#3168=EDGE_LOOP('',(#11748,#11749,#11750,#11751));
#3169=EDGE_LOOP('',(#11752));
#3170=EDGE_LOOP('',(#11753));
#3171=EDGE_LOOP('',(#11754,#11755,#11756,#11757));
#3172=EDGE_LOOP('',(#11758,#11759,#11760,#11761));
#3173=EDGE_LOOP('',(#11762,#11763,#11764,#11765));
#3174=EDGE_LOOP('',(#11766,#11767,#11768,#11769,#11770));
#3175=EDGE_LOOP('',(#11771,#11772,#11773,#11774));
#3176=EDGE_LOOP('',(#11775,#11776));
#3177=EDGE_LOOP('',(#11777,#11778,#11779,#11780));
#3178=EDGE_LOOP('',(#11781,#11782,#11783,#11784));
#3179=EDGE_LOOP('',(#11785,#11786,#11787,#11788));
#3180=EDGE_LOOP('',(#11789));
#3181=EDGE_LOOP('',(#11790));
#3182=EDGE_LOOP('',(#11791));
#3183=EDGE_LOOP('',(#11792));
#3184=EDGE_LOOP('',(#11793,#11794,#11795,#11796));
#3185=EDGE_LOOP('',(#11797,#11798,#11799,#11800));
#3186=EDGE_LOOP('',(#11801));
#3187=EDGE_LOOP('',(#11802));
#3188=EDGE_LOOP('',(#11803));
#3189=EDGE_LOOP('',(#11804));
#3190=EDGE_LOOP('',(#11805,#11806,#11807,#11808,#11809,#11810,#11811,#11812));
#3191=EDGE_LOOP('',(#11813,#11814,#11815,#11816));
#3192=EDGE_LOOP('',(#11817,#11818,#11819,#11820));
#3193=EDGE_LOOP('',(#11821,#11822,#11823,#11824));
#3194=EDGE_LOOP('',(#11825,#11826,#11827,#11828));
#3195=EDGE_LOOP('',(#11829,#11830,#11831,#11832,#11833,#11834,#11835,#11836));
#3196=EDGE_LOOP('',(#11837,#11838,#11839,#11840));
#3197=EDGE_LOOP('',(#11841,#11842,#11843,#11844));
#3198=EDGE_LOOP('',(#11845,#11846,#11847,#11848));
#3199=EDGE_LOOP('',(#11849,#11850,#11851,#11852));
#3200=EDGE_LOOP('',(#11853,#11854,#11855,#11856));
#3201=EDGE_LOOP('',(#11857,#11858,#11859,#11860));
#3202=EDGE_LOOP('',(#11861,#11862,#11863,#11864));
#3203=EDGE_LOOP('',(#11865,#11866,#11867,#11868));
#3204=EDGE_LOOP('',(#11869,#11870,#11871,#11872));
#3205=EDGE_LOOP('',(#11873,#11874,#11875,#11876));
#3206=EDGE_LOOP('',(#11877,#11878,#11879,#11880,#11881,#11882));
#3207=EDGE_LOOP('',(#11883));
#3208=EDGE_LOOP('',(#11884,#11885,#11886,#11887,#11888,#11889));
#3209=EDGE_LOOP('',(#11890,#11891,#11892,#11893));
#3210=EDGE_LOOP('',(#11894,#11895,#11896,#11897));
#3211=EDGE_LOOP('',(#11898,#11899,#11900,#11901));
#3212=EDGE_LOOP('',(#11902));
#3213=EDGE_LOOP('',(#11903,#11904,#11905,#11906));
#3214=EDGE_LOOP('',(#11907,#11908,#11909,#11910));
#3215=EDGE_LOOP('',(#11911));
#3216=EDGE_LOOP('',(#11912));
#3217=EDGE_LOOP('',(#11913));
#3218=EDGE_LOOP('',(#11914));
#3219=EDGE_LOOP('',(#11915));
#3220=EDGE_LOOP('',(#11916,#11917,#11918,#11919));
#3221=EDGE_LOOP('',(#11920,#11921,#11922,#11923));
#3222=EDGE_LOOP('',(#11924,#11925,#11926,#11927));
#3223=EDGE_LOOP('',(#11928));
#3224=EDGE_LOOP('',(#11929));
#3225=EDGE_LOOP('',(#11930,#11931,#11932,#11933));
#3226=EDGE_LOOP('',(#11934,#11935,#11936,#11937));
#3227=EDGE_LOOP('',(#11938,#11939,#11940,#11941));
#3228=EDGE_LOOP('',(#11942));
#3229=EDGE_LOOP('',(#11943,#11944,#11945,#11946));
#3230=EDGE_LOOP('',(#11947,#11948,#11949,#11950));
#3231=EDGE_LOOP('',(#11951,#11952,#11953,#11954));
#3232=EDGE_LOOP('',(#11955,#11956,#11957,#11958));
#3233=EDGE_LOOP('',(#11959,#11960,#11961,#11962));
#3234=EDGE_LOOP('',(#11963,#11964,#11965,#11966));
#3235=EDGE_LOOP('',(#11967,#11968,#11969,#11970,#11971,#11972));
#3236=EDGE_LOOP('',(#11973,#11974,#11975,#11976,#11977,#11978));
#3237=LINE('',#18493,#4171);
#3238=LINE('',#18499,#4172);
#3239=LINE('',#18505,#4173);
#3240=LINE('',#18511,#4174);
#3241=LINE('',#18517,#4175);
#3242=LINE('',#18523,#4176);
#3243=LINE('',#18529,#4177);
#3244=LINE('',#18535,#4178);
#3245=LINE('',#18541,#4179);
#3246=LINE('',#18547,#4180);
#3247=LINE('',#18553,#4181);
#3248=LINE('',#18559,#4182);
#3249=LINE('',#18565,#4183);
#3250=LINE('',#18571,#4184);
#3251=LINE('',#18577,#4185);
#3252=LINE('',#18583,#4186);
#3253=LINE('',#18588,#4187);
#3254=LINE('',#18590,#4188);
#3255=LINE('',#18592,#4189);
#3256=LINE('',#18593,#4190);
#3257=LINE('',#18596,#4191);
#3258=LINE('',#18598,#4192);
#3259=LINE('',#18599,#4193);
#3260=LINE('',#18602,#4194);
#3261=LINE('',#18604,#4195);
#3262=LINE('',#18605,#4196);
#3263=LINE('',#18607,#4197);
#3264=LINE('',#18608,#4198);
#3265=LINE('',#18616,#4199);
#3266=LINE('',#18622,#4200);
#3267=LINE('',#18628,#4201);
#3268=LINE('',#18634,#4202);
#3269=LINE('',#18640,#4203);
#3270=LINE('',#18649,#4204);
#3271=LINE('',#18658,#4205);
#3272=LINE('',#18667,#4206);
#3273=LINE('',#18675,#4207);
#3274=LINE('',#18679,#4208);
#3275=LINE('',#18683,#4209);
#3276=LINE('',#18687,#4210);
#3277=LINE('',#18691,#4211);
#3278=LINE('',#18693,#4212);
#3279=LINE('',#18695,#4213);
#3280=LINE('',#18696,#4214);
#3281=LINE('',#18699,#4215);
#3282=LINE('',#18701,#4216);
#3283=LINE('',#18702,#4217);
#3284=LINE('',#18705,#4218);
#3285=LINE('',#18707,#4219);
#3286=LINE('',#18708,#4220);
#3287=LINE('',#18710,#4221);
#3288=LINE('',#18711,#4222);
#3289=LINE('',#18719,#4223);
#3290=LINE('',#18725,#4224);
#3291=LINE('',#18731,#4225);
#3292=LINE('',#18737,#4226);
#3293=LINE('',#18744,#4227);
#3294=LINE('',#18750,#4228);
#3295=LINE('',#18757,#4229);
#3296=LINE('',#18763,#4230);
#3297=LINE('',#18765,#4231);
#3298=LINE('',#18767,#4232);
#3299=LINE('',#18768,#4233);
#3300=LINE('',#18771,#4234);
#3301=LINE('',#18773,#4235);
#3302=LINE('',#18774,#4236);
#3303=LINE('',#18777,#4237);
#3304=LINE('',#18779,#4238);
#3305=LINE('',#18780,#4239);
#3306=LINE('',#18782,#4240);
#3307=LINE('',#18783,#4241);
#3308=LINE('',#18791,#4242);
#3309=LINE('',#18797,#4243);
#3310=LINE('',#18803,#4244);
#3311=LINE('',#18809,#4245);
#3312=LINE('',#18816,#4246);
#3313=LINE('',#18822,#4247);
#3314=LINE('',#18831,#4248);
#3315=LINE('',#18837,#4249);
#3316=LINE('',#18843,#4250);
#3317=LINE('',#18849,#4251);
#3318=LINE('',#18857,#4252);
#3319=LINE('',#18862,#4253);
#3320=LINE('',#18869,#4254);
#3321=LINE('',#18875,#4255);
#3322=LINE('',#18877,#4256);
#3323=LINE('',#18879,#4257);
#3324=LINE('',#18880,#4258);
#3325=LINE('',#18883,#4259);
#3326=LINE('',#18885,#4260);
#3327=LINE('',#18886,#4261);
#3328=LINE('',#18889,#4262);
#3329=LINE('',#18891,#4263);
#3330=LINE('',#18892,#4264);
#3331=LINE('',#18894,#4265);
#3332=LINE('',#18895,#4266);
#3333=LINE('',#18902,#4267);
#3334=LINE('',#18904,#4268);
#3335=LINE('',#18906,#4269);
#3336=LINE('',#18907,#4270);
#3337=LINE('',#18922,#4271);
#3338=LINE('',#18926,#4272);
#3339=LINE('',#18930,#4273);
#3340=LINE('',#18934,#4274);
#3341=LINE('',#18942,#4275);
#3342=LINE('',#18948,#4276);
#3343=LINE('',#18956,#4277);
#3344=LINE('',#18959,#4278);
#3345=LINE('',#18961,#4279);
#3346=LINE('',#18966,#4280);
#3347=LINE('',#18974,#4281);
#3348=LINE('',#18977,#4282);
#3349=LINE('',#18979,#4283);
#3350=LINE('',#18983,#4284);
#3351=LINE('',#18985,#4285);
#3352=LINE('',#18987,#4286);
#3353=LINE('',#18989,#4287);
#3354=LINE('',#18990,#4288);
#3355=LINE('',#18993,#4289);
#3356=LINE('',#18995,#4290);
#3357=LINE('',#18997,#4291);
#3358=LINE('',#18999,#4292);
#3359=LINE('',#19000,#4293);
#3360=LINE('',#19004,#4294);
#3361=LINE('',#19008,#4295);
#3362=LINE('',#19010,#4296);
#3363=LINE('',#19011,#4297);
#3364=LINE('',#19014,#4298);
#3365=LINE('',#19016,#4299);
#3366=LINE('',#19018,#4300);
#3367=LINE('',#19020,#4301);
#3368=LINE('',#19021,#4302);
#3369=LINE('',#19024,#4303);
#3370=LINE('',#19025,#4304);
#3371=LINE('',#19028,#4305);
#3372=LINE('',#19029,#4306);
#3373=LINE('',#19032,#4307);
#3374=LINE('',#19034,#4308);
#3375=LINE('',#19035,#4309);
#3376=LINE('',#19037,#4310);
#3377=LINE('',#19038,#4311);
#3378=LINE('',#19045,#4312);
#3379=LINE('',#19053,#4313);
#3380=LINE('',#19056,#4314);
#3381=LINE('',#19058,#4315);
#3382=LINE('',#19063,#4316);
#3383=LINE('',#19071,#4317);
#3384=LINE('',#19074,#4318);
#3385=LINE('',#19076,#4319);
#3386=LINE('',#19080,#4320);
#3387=LINE('',#19082,#4321);
#3388=LINE('',#19084,#4322);
#3389=LINE('',#19086,#4323);
#3390=LINE('',#19087,#4324);
#3391=LINE('',#19090,#4325);
#3392=LINE('',#19092,#4326);
#3393=LINE('',#19094,#4327);
#3394=LINE('',#19096,#4328);
#3395=LINE('',#19097,#4329);
#3396=LINE('',#19101,#4330);
#3397=LINE('',#19105,#4331);
#3398=LINE('',#19107,#4332);
#3399=LINE('',#19108,#4333);
#3400=LINE('',#19111,#4334);
#3401=LINE('',#19113,#4335);
#3402=LINE('',#19115,#4336);
#3403=LINE('',#19117,#4337);
#3404=LINE('',#19118,#4338);
#3405=LINE('',#19121,#4339);
#3406=LINE('',#19122,#4340);
#3407=LINE('',#19125,#4341);
#3408=LINE('',#19126,#4342);
#3409=LINE('',#19129,#4343);
#3410=LINE('',#19131,#4344);
#3411=LINE('',#19132,#4345);
#3412=LINE('',#19134,#4346);
#3413=LINE('',#19135,#4347);
#3414=LINE('',#19143,#4348);
#3415=LINE('',#19152,#4349);
#3416=LINE('',#19161,#4350);
#3417=LINE('',#19170,#4351);
#3418=LINE('',#19178,#4352);
#3419=LINE('',#19182,#4353);
#3420=LINE('',#19186,#4354);
#3421=LINE('',#19190,#4355);
#3422=LINE('',#19194,#4356);
#3423=LINE('',#19196,#4357);
#3424=LINE('',#19198,#4358);
#3425=LINE('',#19199,#4359);
#3426=LINE('',#19202,#4360);
#3427=LINE('',#19204,#4361);
#3428=LINE('',#19205,#4362);
#3429=LINE('',#19208,#4363);
#3430=LINE('',#19210,#4364);
#3431=LINE('',#19211,#4365);
#3432=LINE('',#19214,#4366);
#3433=LINE('',#19216,#4367);
#3434=LINE('',#19217,#4368);
#3435=LINE('',#19220,#4369);
#3436=LINE('',#19222,#4370);
#3437=LINE('',#19223,#4371);
#3438=LINE('',#19226,#4372);
#3439=LINE('',#19228,#4373);
#3440=LINE('',#19229,#4374);
#3441=LINE('',#19232,#4375);
#3442=LINE('',#19234,#4376);
#3443=LINE('',#19235,#4377);
#3444=LINE('',#19238,#4378);
#3445=LINE('',#19240,#4379);
#3446=LINE('',#19241,#4380);
#3447=LINE('',#19244,#4381);
#3448=LINE('',#19246,#4382);
#3449=LINE('',#19247,#4383);
#3450=LINE('',#19250,#4384);
#3451=LINE('',#19252,#4385);
#3452=LINE('',#19253,#4386);
#3453=LINE('',#19256,#4387);
#3454=LINE('',#19258,#4388);
#3455=LINE('',#19259,#4389);
#3456=LINE('',#19261,#4390);
#3457=LINE('',#19262,#4391);
#3458=LINE('',#19279,#4392);
#3459=LINE('',#19285,#4393);
#3460=LINE('',#19289,#4394);
#3461=LINE('',#19295,#4395);
#3462=LINE('',#19300,#4396);
#3463=LINE('',#19315,#4397);
#3464=LINE('',#19324,#4398);
#3465=LINE('',#19328,#4399);
#3466=LINE('',#19332,#4400);
#3467=LINE('',#19335,#4401);
#3468=LINE('',#19471,#4402);
#3469=LINE('',#19724,#4403);
#3470=LINE('',#19766,#4404);
#3471=LINE('',#19771,#4405);
#3472=LINE('',#19780,#4406);
#3473=LINE('',#19785,#4407);
#3474=LINE('',#19805,#4408);
#3475=LINE('',#19811,#4409);
#3476=LINE('',#19815,#4410);
#3477=LINE('',#19821,#4411);
#3478=LINE('',#19826,#4412);
#3479=LINE('',#19841,#4413);
#3480=LINE('',#19850,#4414);
#3481=LINE('',#19854,#4415);
#3482=LINE('',#19858,#4416);
#3483=LINE('',#19861,#4417);
#3484=LINE('',#20014,#4418);
#3485=LINE('',#20310,#4419);
#3486=LINE('',#20352,#4420);
#3487=LINE('',#20357,#4421);
#3488=LINE('',#20366,#4422);
#3489=LINE('',#20371,#4423);
#3490=LINE('',#20381,#4424);
#3491=LINE('',#20383,#4425);
#3492=LINE('',#20385,#4426);
#3493=LINE('',#20386,#4427);
#3494=LINE('',#20389,#4428);
#3495=LINE('',#20391,#4429);
#3496=LINE('',#20392,#4430);
#3497=LINE('',#20395,#4431);
#3498=LINE('',#20397,#4432);
#3499=LINE('',#20398,#4433);
#3500=LINE('',#20401,#4434);
#3501=LINE('',#20403,#4435);
#3502=LINE('',#20404,#4436);
#3503=LINE('',#20407,#4437);
#3504=LINE('',#20409,#4438);
#3505=LINE('',#20410,#4439);
#3506=LINE('',#20413,#4440);
#3507=LINE('',#20415,#4441);
#3508=LINE('',#20416,#4442);
#3509=LINE('',#20419,#4443);
#3510=LINE('',#20421,#4444);
#3511=LINE('',#20422,#4445);
#3512=LINE('',#20425,#4446);
#3513=LINE('',#20427,#4447);
#3514=LINE('',#20428,#4448);
#3515=LINE('',#20431,#4449);
#3516=LINE('',#20433,#4450);
#3517=LINE('',#20434,#4451);
#3518=LINE('',#20438,#4452);
#3519=LINE('',#20440,#4453);
#3520=LINE('',#20442,#4454);
#3521=LINE('',#20443,#4455);
#3522=LINE('',#20446,#4456);
#3523=LINE('',#20448,#4457);
#3524=LINE('',#20449,#4458);
#3525=LINE('',#20452,#4459);
#3526=LINE('',#20454,#4460);
#3527=LINE('',#20455,#4461);
#3528=LINE('',#20458,#4462);
#3529=LINE('',#20460,#4463);
#3530=LINE('',#20461,#4464);
#3531=LINE('',#20464,#4465);
#3532=LINE('',#20466,#4466);
#3533=LINE('',#20467,#4467);
#3534=LINE('',#20470,#4468);
#3535=LINE('',#20472,#4469);
#3536=LINE('',#20473,#4470);
#3537=LINE('',#20476,#4471);
#3538=LINE('',#20478,#4472);
#3539=LINE('',#20479,#4473);
#3540=LINE('',#20482,#4474);
#3541=LINE('',#20484,#4475);
#3542=LINE('',#20485,#4476);
#3543=LINE('',#20488,#4477);
#3544=LINE('',#20490,#4478);
#3545=LINE('',#20491,#4479);
#3546=LINE('',#20495,#4480);
#3547=LINE('',#20497,#4481);
#3548=LINE('',#20499,#4482);
#3549=LINE('',#20500,#4483);
#3550=LINE('',#20503,#4484);
#3551=LINE('',#20505,#4485);
#3552=LINE('',#20506,#4486);
#3553=LINE('',#20509,#4487);
#3554=LINE('',#20511,#4488);
#3555=LINE('',#20512,#4489);
#3556=LINE('',#20515,#4490);
#3557=LINE('',#20517,#4491);
#3558=LINE('',#20518,#4492);
#3559=LINE('',#20521,#4493);
#3560=LINE('',#20523,#4494);
#3561=LINE('',#20524,#4495);
#3562=LINE('',#20527,#4496);
#3563=LINE('',#20529,#4497);
#3564=LINE('',#20530,#4498);
#3565=LINE('',#20533,#4499);
#3566=LINE('',#20535,#4500);
#3567=LINE('',#20536,#4501);
#3568=LINE('',#20539,#4502);
#3569=LINE('',#20541,#4503);
#3570=LINE('',#20542,#4504);
#3571=LINE('',#20545,#4505);
#3572=LINE('',#20547,#4506);
#3573=LINE('',#20548,#4507);
#3574=LINE('',#20552,#4508);
#3575=LINE('',#20554,#4509);
#3576=LINE('',#20556,#4510);
#3577=LINE('',#20557,#4511);
#3578=LINE('',#20560,#4512);
#3579=LINE('',#20562,#4513);
#3580=LINE('',#20563,#4514);
#3581=LINE('',#20566,#4515);
#3582=LINE('',#20568,#4516);
#3583=LINE('',#20569,#4517);
#3584=LINE('',#20572,#4518);
#3585=LINE('',#20574,#4519);
#3586=LINE('',#20575,#4520);
#3587=LINE('',#20578,#4521);
#3588=LINE('',#20580,#4522);
#3589=LINE('',#20581,#4523);
#3590=LINE('',#20584,#4524);
#3591=LINE('',#20586,#4525);
#3592=LINE('',#20587,#4526);
#3593=LINE('',#20590,#4527);
#3594=LINE('',#20592,#4528);
#3595=LINE('',#20593,#4529);
#3596=LINE('',#20596,#4530);
#3597=LINE('',#20598,#4531);
#3598=LINE('',#20599,#4532);
#3599=LINE('',#20602,#4533);
#3600=LINE('',#20604,#4534);
#3601=LINE('',#20605,#4535);
#3602=LINE('',#20610,#4536);
#3603=LINE('',#20614,#4537);
#3604=LINE('',#20616,#4538);
#3605=LINE('',#20617,#4539);
#3606=LINE('',#20620,#4540);
#3607=LINE('',#20622,#4541);
#3608=LINE('',#20623,#4542);
#3609=LINE('',#20625,#4543);
#3610=LINE('',#20626,#4544);
#3611=LINE('',#20629,#4545);
#3612=LINE('',#20631,#4546);
#3613=LINE('',#20632,#4547);
#3614=LINE('',#20634,#4548);
#3615=LINE('',#20635,#4549);
#3616=LINE('',#20638,#4550);
#3617=LINE('',#20640,#4551);
#3618=LINE('',#20641,#4552);
#3619=LINE('',#20643,#4553);
#3620=LINE('',#20644,#4554);
#3621=LINE('',#20646,#4555);
#3622=LINE('',#20647,#4556);
#3623=LINE('',#20654,#4557);
#3624=LINE('',#20656,#4558);
#3625=LINE('',#20658,#4559);
#3626=LINE('',#20660,#4560);
#3627=LINE('',#20663,#4561);
#3628=LINE('',#20668,#4562);
#3629=LINE('',#20677,#4563);
#3630=LINE('',#20678,#4564);
#3631=LINE('',#20681,#4565);
#3632=LINE('',#20682,#4566);
#3633=LINE('',#20685,#4567);
#3634=LINE('',#20687,#4568);
#3635=LINE('',#20688,#4569);
#3636=LINE('',#20691,#4570);
#3637=LINE('',#20693,#4571);
#3638=LINE('',#20694,#4572);
#3639=LINE('',#20697,#4573);
#3640=LINE('',#20698,#4574);
#3641=LINE('',#20701,#4575);
#3642=LINE('',#20702,#4576);
#3643=LINE('',#20704,#4577);
#3644=LINE('',#20711,#4578);
#3645=LINE('',#20715,#4579);
#3646=LINE('',#20722,#4580);
#3647=LINE('',#20729,#4581);
#3648=LINE('',#20731,#4582);
#3649=LINE('',#20733,#4583);
#3650=LINE('',#20734,#4584);
#3651=LINE('',#20737,#4585);
#3652=LINE('',#20739,#4586);
#3653=LINE('',#20740,#4587);
#3654=LINE('',#20743,#4588);
#3655=LINE('',#20745,#4589);
#3656=LINE('',#20746,#4590);
#3657=LINE('',#20749,#4591);
#3658=LINE('',#20751,#4592);
#3659=LINE('',#20752,#4593);
#3660=LINE('',#20755,#4594);
#3661=LINE('',#20757,#4595);
#3662=LINE('',#20758,#4596);
#3663=LINE('',#20760,#4597);
#3664=LINE('',#20761,#4598);
#3665=LINE('',#20773,#4599);
#3666=LINE('',#20777,#4600);
#3667=LINE('',#20781,#4601);
#3668=LINE('',#20788,#4602);
#3669=LINE('',#20790,#4603);
#3670=LINE('',#20797,#4604);
#3671=LINE('',#20803,#4605);
#3672=LINE('',#20809,#4606);
#3673=LINE('',#20815,#4607);
#3674=LINE('',#20820,#4608);
#3675=LINE('',#20822,#4609);
#3676=LINE('',#20824,#4610);
#3677=LINE('',#20825,#4611);
#3678=LINE('',#20828,#4612);
#3679=LINE('',#20830,#4613);
#3680=LINE('',#20831,#4614);
#3681=LINE('',#20834,#4615);
#3682=LINE('',#20836,#4616);
#3683=LINE('',#20837,#4617);
#3684=LINE('',#20839,#4618);
#3685=LINE('',#20840,#4619);
#3686=LINE('',#20848,#4620);
#3687=LINE('',#20854,#4621);
#3688=LINE('',#20860,#4622);
#3689=LINE('',#20866,#4623);
#3690=LINE('',#20872,#4624);
#3691=LINE('',#20878,#4625);
#3692=LINE('',#20884,#4626);
#3693=LINE('',#20890,#4627);
#3694=LINE('',#20895,#4628);
#3695=LINE('',#20897,#4629);
#3696=LINE('',#20899,#4630);
#3697=LINE('',#20900,#4631);
#3698=LINE('',#20903,#4632);
#3699=LINE('',#20905,#4633);
#3700=LINE('',#20906,#4634);
#3701=LINE('',#20909,#4635);
#3702=LINE('',#20911,#4636);
#3703=LINE('',#20912,#4637);
#3704=LINE('',#20914,#4638);
#3705=LINE('',#20915,#4639);
#3706=LINE('',#20923,#4640);
#3707=LINE('',#20930,#4641);
#3708=LINE('',#20937,#4642);
#3709=LINE('',#20944,#4643);
#3710=LINE('',#20951,#4644);
#3711=LINE('',#20958,#4645);
#3712=LINE('',#20965,#4646);
#3713=LINE('',#20972,#4647);
#3714=LINE('',#20977,#4648);
#3715=LINE('',#20979,#4649);
#3716=LINE('',#20981,#4650);
#3717=LINE('',#20982,#4651);
#3718=LINE('',#20985,#4652);
#3719=LINE('',#20987,#4653);
#3720=LINE('',#20988,#4654);
#3721=LINE('',#20991,#4655);
#3722=LINE('',#20993,#4656);
#3723=LINE('',#20994,#4657);
#3724=LINE('',#20996,#4658);
#3725=LINE('',#20997,#4659);
#3726=LINE('',#21005,#4660);
#3727=LINE('',#21009,#4661);
#3728=LINE('',#21013,#4662);
#3729=LINE('',#21017,#4663);
#3730=LINE('',#21021,#4664);
#3731=LINE('',#21025,#4665);
#3732=LINE('',#21029,#4666);
#3733=LINE('',#21033,#4667);
#3734=LINE('',#21037,#4668);
#3735=LINE('',#21041,#4669);
#3736=LINE('',#21045,#4670);
#3737=LINE('',#21049,#4671);
#3738=LINE('',#21053,#4672);
#3739=LINE('',#21057,#4673);
#3740=LINE('',#21061,#4674);
#3741=LINE('',#21065,#4675);
#3742=LINE('',#21067,#4676);
#3743=LINE('',#21069,#4677);
#3744=LINE('',#21071,#4678);
#3745=LINE('',#21073,#4679);
#3746=LINE('',#21075,#4680);
#3747=LINE('',#21076,#4681);
#3748=LINE('',#21078,#4682);
#3749=LINE('',#21080,#4683);
#3750=LINE('',#21082,#4684);
#3751=LINE('',#21084,#4685);
#3752=LINE('',#21086,#4686);
#3753=LINE('',#21087,#4687);
#3754=LINE('',#21090,#4688);
#3755=LINE('',#21092,#4689);
#3756=LINE('',#21094,#4690);
#3757=LINE('',#21096,#4691);
#3758=LINE('',#21097,#4692);
#3759=LINE('',#21099,#4693);
#3760=LINE('',#21101,#4694);
#3761=LINE('',#21103,#4695);
#3762=LINE('',#21105,#4696);
#3763=LINE('',#21106,#4697);
#3764=LINE('',#21109,#4698);
#3765=LINE('',#21110,#4699);
#3766=LINE('',#21113,#4700);
#3767=LINE('',#21114,#4701);
#3768=LINE('',#21117,#4702);
#3769=LINE('',#21118,#4703);
#3770=LINE('',#21121,#4704);
#3771=LINE('',#21122,#4705);
#3772=LINE('',#21124,#4706);
#3773=LINE('',#21127,#4707);
#3774=LINE('',#21128,#4708);
#3775=LINE('',#21131,#4709);
#3776=LINE('',#21132,#4710);
#3777=LINE('',#21135,#4711);
#3778=LINE('',#21136,#4712);
#3779=LINE('',#21139,#4713);
#3780=LINE('',#21140,#4714);
#3781=LINE('',#21142,#4715);
#3782=LINE('',#21148,#4716);
#3783=LINE('',#21150,#4717);
#3784=LINE('',#21152,#4718);
#3785=LINE('',#21153,#4719);
#3786=LINE('',#21156,#4720);
#3787=LINE('',#21158,#4721);
#3788=LINE('',#21159,#4722);
#3789=LINE('',#21162,#4723);
#3790=LINE('',#21164,#4724);
#3791=LINE('',#21165,#4725);
#3792=LINE('',#21168,#4726);
#3793=LINE('',#21170,#4727);
#3794=LINE('',#21171,#4728);
#3795=LINE('',#21174,#4729);
#3796=LINE('',#21176,#4730);
#3797=LINE('',#21177,#4731);
#3798=LINE('',#21180,#4732);
#3799=LINE('',#21182,#4733);
#3800=LINE('',#21183,#4734);
#3801=LINE('',#21186,#4735);
#3802=LINE('',#21188,#4736);
#3803=LINE('',#21189,#4737);
#3804=LINE('',#21191,#4738);
#3805=LINE('',#21192,#4739);
#3806=LINE('',#21199,#4740);
#3807=LINE('',#21201,#4741);
#3808=LINE('',#21203,#4742);
#3809=LINE('',#21204,#4743);
#3810=LINE('',#21207,#4744);
#3811=LINE('',#21209,#4745);
#3812=LINE('',#21210,#4746);
#3813=LINE('',#21213,#4747);
#3814=LINE('',#21215,#4748);
#3815=LINE('',#21216,#4749);
#3816=LINE('',#21219,#4750);
#3817=LINE('',#21221,#4751);
#3818=LINE('',#21222,#4752);
#3819=LINE('',#21225,#4753);
#3820=LINE('',#21227,#4754);
#3821=LINE('',#21228,#4755);
#3822=LINE('',#21231,#4756);
#3823=LINE('',#21233,#4757);
#3824=LINE('',#21234,#4758);
#3825=LINE('',#21237,#4759);
#3826=LINE('',#21239,#4760);
#3827=LINE('',#21240,#4761);
#3828=LINE('',#21242,#4762);
#3829=LINE('',#21243,#4763);
#3830=LINE('',#21254,#4764);
#3831=LINE('',#21258,#4765);
#3832=LINE('',#21265,#4766);
#3833=LINE('',#21272,#4767);
#3834=LINE('',#21274,#4768);
#3835=LINE('',#21276,#4769);
#3836=LINE('',#21277,#4770);
#3837=LINE('',#21280,#4771);
#3838=LINE('',#21282,#4772);
#3839=LINE('',#21283,#4773);
#3840=LINE('',#21286,#4774);
#3841=LINE('',#21288,#4775);
#3842=LINE('',#21289,#4776);
#3843=LINE('',#21292,#4777);
#3844=LINE('',#21294,#4778);
#3845=LINE('',#21295,#4779);
#3846=LINE('',#21298,#4780);
#3847=LINE('',#21300,#4781);
#3848=LINE('',#21301,#4782);
#3849=LINE('',#21303,#4783);
#3850=LINE('',#21304,#4784);
#3851=LINE('',#21314,#4785);
#3852=LINE('',#21323,#4786);
#3853=LINE('',#21327,#4787);
#3854=LINE('',#21331,#4788);
#3855=LINE('',#21338,#4789);
#3856=LINE('',#21340,#4790);
#3857=LINE('',#21345,#4791);
#3858=LINE('',#21417,#4792);
#3859=LINE('',#21504,#4793);
#3860=LINE('',#21594,#4794);
#3861=LINE('',#21681,#4795);
#3862=LINE('',#21771,#4796);
#3863=LINE('',#21858,#4797);
#3864=LINE('',#21945,#4798);
#3865=LINE('',#22035,#4799);
#3866=LINE('',#22051,#4800);
#3867=LINE('',#22077,#4801);
#3868=LINE('',#22114,#4802);
#3869=LINE('',#22151,#4803);
#3870=LINE('',#22189,#4804);
#3871=LINE('',#22226,#4805);
#3872=LINE('',#22263,#4806);
#3873=LINE('',#22301,#4807);
#3874=LINE('',#22339,#4808);
#3875=LINE('',#23504,#4809);
#3876=LINE('',#23516,#4810);
#3877=LINE('',#23520,#4811);
#3878=LINE('',#23524,#4812);
#3879=LINE('',#23528,#4813);
#3880=LINE('',#23529,#4814);
#3881=LINE('',#23530,#4815);
#3882=LINE('',#23539,#4816);
#3883=LINE('',#23549,#4817);
#3884=LINE('',#23553,#4818);
#3885=LINE('',#23557,#4819);
#3886=LINE('',#23564,#4820);
#3887=LINE('',#23568,#4821);
#3888=LINE('',#23572,#4822);
#3889=LINE('',#23577,#4823);
#3890=LINE('',#23579,#4824);
#3891=LINE('',#23581,#4825);
#3892=LINE('',#23582,#4826);
#3893=LINE('',#23585,#4827);
#3894=LINE('',#23587,#4828);
#3895=LINE('',#23588,#4829);
#3896=LINE('',#23591,#4830);
#3897=LINE('',#23593,#4831);
#3898=LINE('',#23594,#4832);
#3899=LINE('',#23597,#4833);
#3900=LINE('',#23599,#4834);
#3901=LINE('',#23600,#4835);
#3902=LINE('',#23603,#4836);
#3903=LINE('',#23605,#4837);
#3904=LINE('',#23606,#4838);
#3905=LINE('',#23608,#4839);
#3906=LINE('',#23609,#4840);
#3907=LINE('',#23619,#4841);
#3908=LINE('',#23623,#4842);
#3909=LINE('',#23627,#4843);
#3910=LINE('',#23634,#4844);
#3911=LINE('',#23638,#4845);
#3912=LINE('',#23642,#4846);
#3913=LINE('',#23647,#4847);
#3914=LINE('',#23649,#4848);
#3915=LINE('',#23651,#4849);
#3916=LINE('',#23652,#4850);
#3917=LINE('',#23655,#4851);
#3918=LINE('',#23657,#4852);
#3919=LINE('',#23658,#4853);
#3920=LINE('',#23661,#4854);
#3921=LINE('',#23663,#4855);
#3922=LINE('',#23664,#4856);
#3923=LINE('',#23667,#4857);
#3924=LINE('',#23669,#4858);
#3925=LINE('',#23670,#4859);
#3926=LINE('',#23673,#4860);
#3927=LINE('',#23675,#4861);
#3928=LINE('',#23676,#4862);
#3929=LINE('',#23678,#4863);
#3930=LINE('',#23679,#4864);
#3931=LINE('',#23707,#4865);
#3932=LINE('',#23737,#4866);
#3933=LINE('',#23824,#4867);
#3934=LINE('',#23914,#4868);
#3935=LINE('',#24001,#4869);
#3936=LINE('',#24088,#4870);
#3937=LINE('',#24175,#4871);
#3938=LINE('',#24262,#4872);
#3939=LINE('',#24349,#4873);
#3940=LINE('',#24421,#4874);
#3941=LINE('',#24472,#4875);
#3942=LINE('',#24520,#4876);
#3943=LINE('',#24568,#4877);
#3944=LINE('',#24619,#4878);
#3945=LINE('',#24670,#4879);
#3946=LINE('',#24718,#4880);
#3947=LINE('',#24769,#4881);
#3948=LINE('',#24820,#4882);
#3949=LINE('',#24868,#4883);
#3950=LINE('',#24916,#4884);
#3951=LINE('',#24967,#4885);
#3952=LINE('',#25018,#4886);
#3953=LINE('',#25066,#4887);
#3954=LINE('',#25117,#4888);
#3955=LINE('',#25168,#4889);
#3956=LINE('',#25216,#4890);
#3957=LINE('',#25264,#4891);
#3958=LINE('',#25315,#4892);
#3959=LINE('',#25366,#4893);
#3960=LINE('',#25414,#4894);
#3961=LINE('',#25465,#4895);
#3962=LINE('',#25516,#4896);
#3963=LINE('',#25564,#4897);
#3964=LINE('',#25612,#4898);
#3965=LINE('',#25663,#4899);
#3966=LINE('',#25714,#4900);
#3967=LINE('',#25762,#4901);
#3968=LINE('',#25813,#4902);
#3969=LINE('',#25864,#4903);
#3970=LINE('',#25912,#4904);
#3971=LINE('',#25960,#4905);
#3972=LINE('',#26011,#4906);
#3973=LINE('',#26062,#4907);
#3974=LINE('',#26110,#4908);
#3975=LINE('',#26161,#4909);
#3976=LINE('',#26212,#4910);
#3977=LINE('',#26260,#4911);
#3978=LINE('',#26308,#4912);
#3979=LINE('',#26359,#4913);
#3980=LINE('',#26410,#4914);
#3981=LINE('',#26458,#4915);
#3982=LINE('',#26509,#4916);
#3983=LINE('',#26560,#4917);
#3984=LINE('',#26608,#4918);
#3985=LINE('',#26656,#4919);
#3986=LINE('',#26707,#4920);
#3987=LINE('',#26773,#4921);
#3988=LINE('',#26863,#4922);
#3989=LINE('',#26950,#4923);
#3990=LINE('',#27037,#4924);
#3991=LINE('',#27124,#4925);
#3992=LINE('',#27211,#4926);
#3993=LINE('',#27298,#4927);
#3994=LINE('',#27388,#4928);
#3995=LINE('',#27398,#4929);
#3996=LINE('',#27434,#4930);
#3997=LINE('',#27472,#4931);
#3998=LINE('',#27508,#4932);
#3999=LINE('',#27546,#4933);
#4000=LINE('',#27582,#4934);
#4001=LINE('',#27620,#4935);
#4002=LINE('',#27657,#4936);
#4003=LINE('',#27692,#4937);
#4004=LINE('',#27719,#4938);
#4005=LINE('',#27743,#4939);
#4006=LINE('',#27767,#4940);
#4007=LINE('',#27791,#4941);
#4008=LINE('',#27817,#4942);
#4009=LINE('',#27841,#4943);
#4010=LINE('',#27865,#4944);
#4011=LINE('',#27891,#4945);
#4012=LINE('',#27915,#4946);
#4013=LINE('',#27939,#4947);
#4014=LINE('',#27963,#4948);
#4015=LINE('',#27989,#4949);
#4016=LINE('',#28013,#4950);
#4017=LINE('',#28037,#4951);
#4018=LINE('',#28063,#4952);
#4019=LINE('',#28087,#4953);
#4020=LINE('',#28111,#4954);
#4021=LINE('',#28135,#4955);
#4022=LINE('',#28161,#4956);
#4023=LINE('',#28185,#4957);
#4024=LINE('',#28209,#4958);
#4025=LINE('',#28235,#4959);
#4026=LINE('',#28259,#4960);
#4027=LINE('',#28283,#4961);
#4028=LINE('',#28307,#4962);
#4029=LINE('',#28333,#4963);
#4030=LINE('',#28357,#4964);
#4031=LINE('',#28381,#4965);
#4032=LINE('',#28407,#4966);
#4033=LINE('',#28431,#4967);
#4034=LINE('',#28455,#4968);
#4035=LINE('',#28479,#4969);
#4036=LINE('',#28505,#4970);
#4037=LINE('',#28529,#4971);
#4038=LINE('',#28553,#4972);
#4039=LINE('',#28579,#4973);
#4040=LINE('',#28603,#4974);
#4041=LINE('',#28627,#4975);
#4042=LINE('',#28651,#4976);
#4043=LINE('',#28677,#4977);
#4044=LINE('',#28701,#4978);
#4045=LINE('',#28725,#4979);
#4046=LINE('',#28751,#4980);
#4047=LINE('',#28775,#4981);
#4048=LINE('',#28799,#4982);
#4049=LINE('',#28824,#4983);
#4050=LINE('',#28851,#4984);
#4051=LINE('',#28888,#4985);
#4052=LINE('',#28924,#4986);
#4053=LINE('',#28962,#4987);
#4054=LINE('',#28998,#4988);
#4055=LINE('',#29036,#4989);
#4056=LINE('',#29073,#4990);
#4057=LINE('',#29189,#4991);
#4058=LINE('',#33323,#4992);
#4059=LINE('',#33325,#4993);
#4060=LINE('',#33327,#4994);
#4061=LINE('',#33328,#4995);
#4062=LINE('',#33333,#4996);
#4063=LINE('',#33334,#4997);
#4064=LINE('',#33337,#4998);
#4065=LINE('',#33338,#4999);
#4066=LINE('',#33341,#5000);
#4067=LINE('',#33342,#5001);
#4068=LINE('',#33349,#5002);
#4069=LINE('',#33359,#5003);
#4070=LINE('',#33367,#5004);
#4071=LINE('',#33373,#5005);
#4072=LINE('',#33381,#5006);
#4073=LINE('',#33419,#5007);
#4074=LINE('',#33458,#5008);
#4075=LINE('',#33463,#5009);
#4076=LINE('',#33469,#5010);
#4077=LINE('',#33478,#5011);
#4078=LINE('',#33483,#5012);
#4079=LINE('',#33513,#5013);
#4080=LINE('',#33552,#5014);
#4081=LINE('',#33556,#5015);
#4082=LINE('',#33558,#5016);
#4083=LINE('',#33560,#5017);
#4084=LINE('',#33562,#5018);
#4085=LINE('',#33564,#5019);
#4086=LINE('',#33565,#5020);
#4087=LINE('',#33568,#5021);
#4088=LINE('',#33570,#5022);
#4089=LINE('',#33571,#5023);
#4090=LINE('',#33574,#5024);
#4091=LINE('',#33576,#5025);
#4092=LINE('',#33578,#5026);
#4093=LINE('',#33580,#5027);
#4094=LINE('',#33581,#5028);
#4095=LINE('',#33591,#5029);
#4096=LINE('',#33602,#5030);
#4097=LINE('',#33608,#5031);
#4098=LINE('',#33617,#5032);
#4099=LINE('',#33623,#5033);
#4100=LINE('',#33631,#5034);
#4101=LINE('',#33633,#5035);
#4102=LINE('',#33635,#5036);
#4103=LINE('',#33637,#5037);
#4104=LINE('',#33639,#5038);
#4105=LINE('',#33641,#5039);
#4106=LINE('',#33643,#5040);
#4107=LINE('',#33644,#5041);
#4108=LINE('',#33647,#5042);
#4109=LINE('',#33649,#5043);
#4110=LINE('',#33650,#5044);
#4111=LINE('',#33653,#5045);
#4112=LINE('',#33654,#5046);
#4113=LINE('',#33657,#5047);
#4114=LINE('',#33658,#5048);
#4115=LINE('',#33661,#5049);
#4116=LINE('',#33662,#5050);
#4117=LINE('',#33666,#5051);
#4118=LINE('',#33667,#5052);
#4119=LINE('',#33669,#5053);
#4120=LINE('',#33670,#5054);
#4121=LINE('',#33672,#5055);
#4122=LINE('',#33674,#5056);
#4123=LINE('',#33676,#5057);
#4124=LINE('',#33682,#5058);
#4125=LINE('',#33684,#5059);
#4126=LINE('',#33686,#5060);
#4127=LINE('',#33687,#5061);
#4128=LINE('',#33690,#5062);
#4129=LINE('',#33692,#5063);
#4130=LINE('',#33693,#5064);
#4131=LINE('',#33696,#5065);
#4132=LINE('',#33698,#5066);
#4133=LINE('',#33699,#5067);
#4134=LINE('',#33702,#5068);
#4135=LINE('',#33704,#5069);
#4136=LINE('',#33705,#5070);
#4137=LINE('',#33708,#5071);
#4138=LINE('',#33710,#5072);
#4139=LINE('',#33711,#5073);
#4140=LINE('',#33713,#5074);
#4141=LINE('',#33714,#5075);
#4142=LINE('',#33722,#5076);
#4143=LINE('',#33726,#5077);
#4144=LINE('',#33730,#5078);
#4145=LINE('',#33737,#5079);
#4146=LINE('',#33743,#5080);
#4147=LINE('',#33754,#5081);
#4148=LINE('',#33758,#5082);
#4149=LINE('',#33762,#5083);
#4150=LINE('',#33769,#5084);
#4151=LINE('',#33773,#5085);
#4152=LINE('',#33777,#5086);
#4153=LINE('',#33782,#5087);
#4154=LINE('',#33784,#5088);
#4155=LINE('',#33786,#5089);
#4156=LINE('',#33787,#5090);
#4157=LINE('',#33790,#5091);
#4158=LINE('',#33792,#5092);
#4159=LINE('',#33793,#5093);
#4160=LINE('',#33796,#5094);
#4161=LINE('',#33798,#5095);
#4162=LINE('',#33799,#5096);
#4163=LINE('',#33802,#5097);
#4164=LINE('',#33804,#5098);
#4165=LINE('',#33805,#5099);
#4166=LINE('',#33808,#5100);
#4167=LINE('',#33810,#5101);
#4168=LINE('',#33811,#5102);
#4169=LINE('',#33813,#5103);
#4170=LINE('',#33814,#5104);
#4171=VECTOR('',#14900,0.274999999999999);
#4172=VECTOR('',#14907,0.275);
#4173=VECTOR('',#14914,0.275);
#4174=VECTOR('',#14921,0.274999999999999);
#4175=VECTOR('',#14928,0.210000000000001);
#4176=VECTOR('',#14935,0.210000000000001);
#4177=VECTOR('',#14942,0.21);
#4178=VECTOR('',#14949,0.21);
#4179=VECTOR('',#14956,0.329999999999998);
#4180=VECTOR('',#14963,0.329999999999998);
#4181=VECTOR('',#14970,0.275);
#4182=VECTOR('',#14977,0.275);
#4183=VECTOR('',#14984,0.210000000000001);
#4184=VECTOR('',#14991,0.21);
#4185=VECTOR('',#14998,0.21);
#4186=VECTOR('',#15005,0.210000000000001);
#4187=VECTOR('',#15010,1.);
#4188=VECTOR('',#15011,1.);
#4189=VECTOR('',#15012,1.);
#4190=VECTOR('',#15013,1.);
#4191=VECTOR('',#15016,1.);
#4192=VECTOR('',#15017,1.);
#4193=VECTOR('',#15018,1.);
#4194=VECTOR('',#15021,1.);
#4195=VECTOR('',#15022,1.);
#4196=VECTOR('',#15023,1.);
#4197=VECTOR('',#15026,1.);
#4198=VECTOR('',#15027,1.);
#4199=VECTOR('',#15038,0.164999999999999);
#4200=VECTOR('',#15045,0.164999999999999);
#4201=VECTOR('',#15052,0.165);
#4202=VECTOR('',#15059,0.164999999999999);
#4203=VECTOR('',#15066,0.5);
#4204=VECTOR('',#15077,0.5);
#4205=VECTOR('',#15088,0.5);
#4206=VECTOR('',#15099,0.5);
#4207=VECTOR('',#15110,0.274999999999999);
#4208=VECTOR('',#15115,0.275);
#4209=VECTOR('',#15120,0.275);
#4210=VECTOR('',#15125,0.274999999999999);
#4211=VECTOR('',#15128,1.);
#4212=VECTOR('',#15129,1.);
#4213=VECTOR('',#15130,1.);
#4214=VECTOR('',#15131,1.);
#4215=VECTOR('',#15134,1.);
#4216=VECTOR('',#15135,1.);
#4217=VECTOR('',#15136,1.);
#4218=VECTOR('',#15139,1.);
#4219=VECTOR('',#15140,1.);
#4220=VECTOR('',#15141,1.);
#4221=VECTOR('',#15144,1.);
#4222=VECTOR('',#15145,1.);
#4223=VECTOR('',#15156,0.165);
#4224=VECTOR('',#15163,0.165);
#4225=VECTOR('',#15170,0.165);
#4226=VECTOR('',#15177,1.6);
#4227=VECTOR('',#15186,1.4);
#4228=VECTOR('',#15193,0.21);
#4229=VECTOR('',#15202,0.21);
#4230=VECTOR('',#15209,1.);
#4231=VECTOR('',#15210,1.);
#4232=VECTOR('',#15211,1.);
#4233=VECTOR('',#15212,1.);
#4234=VECTOR('',#15215,1.);
#4235=VECTOR('',#15216,1.);
#4236=VECTOR('',#15217,1.);
#4237=VECTOR('',#15220,1.);
#4238=VECTOR('',#15221,1.);
#4239=VECTOR('',#15222,1.);
#4240=VECTOR('',#15225,1.);
#4241=VECTOR('',#15226,1.);
#4242=VECTOR('',#15237,0.225);
#4243=VECTOR('',#15244,0.225);
#4244=VECTOR('',#15251,0.225);
#4245=VECTOR('',#15258,1.59);
#4246=VECTOR('',#15267,1.2);
#4247=VECTOR('',#15274,2.4);
#4248=VECTOR('',#15287,0.165);
#4249=VECTOR('',#15294,0.165);
#4250=VECTOR('',#15301,0.165);
#4251=VECTOR('',#15308,2.35);
#4252=VECTOR('',#15319,2.15);
#4253=VECTOR('',#15324,0.25);
#4254=VECTOR('',#15333,0.25);
#4255=VECTOR('',#15340,1.);
#4256=VECTOR('',#15341,1.);
#4257=VECTOR('',#15342,1.);
#4258=VECTOR('',#15343,1.);
#4259=VECTOR('',#15346,1.);
#4260=VECTOR('',#15347,1.);
#4261=VECTOR('',#15348,1.);
#4262=VECTOR('',#15351,1.);
#4263=VECTOR('',#15352,1.);
#4264=VECTOR('',#15353,1.);
#4265=VECTOR('',#15356,1.);
#4266=VECTOR('',#15357,1.);
#4267=VECTOR('',#15366,1.);
#4268=VECTOR('',#15367,1.);
#4269=VECTOR('',#15368,1.);
#4270=VECTOR('',#15369,1.);
#4271=VECTOR('',#15388,0.225);
#4272=VECTOR('',#15393,0.225);
#4273=VECTOR('',#15398,0.225);
#4274=VECTOR('',#15403,2.34);
#4275=VECTOR('',#15414,1.8);
#4276=VECTOR('',#15421,1.);
#4277=VECTOR('',#15430,1.);
#4278=VECTOR('',#15433,1.);
#4279=VECTOR('',#15434,0.475);
#4280=VECTOR('',#15439,1.);
#4281=VECTOR('',#15448,1.);
#4282=VECTOR('',#15451,1.);
#4283=VECTOR('',#15452,0.475);
#4284=VECTOR('',#15457,1.);
#4285=VECTOR('',#15458,1.);
#4286=VECTOR('',#15459,1.);
#4287=VECTOR('',#15460,1.);
#4288=VECTOR('',#15461,1.);
#4289=VECTOR('',#15464,1.);
#4290=VECTOR('',#15465,1.);
#4291=VECTOR('',#15466,1.);
#4292=VECTOR('',#15467,1.);
#4293=VECTOR('',#15468,1.);
#4294=VECTOR('',#15473,0.275);
#4295=VECTOR('',#15478,0.275);
#4296=VECTOR('',#15481,1.);
#4297=VECTOR('',#15482,1.);
#4298=VECTOR('',#15485,1.);
#4299=VECTOR('',#15486,1.);
#4300=VECTOR('',#15487,1.);
#4301=VECTOR('',#15488,1.);
#4302=VECTOR('',#15489,1.);
#4303=VECTOR('',#15492,1.);
#4304=VECTOR('',#15493,1.);
#4305=VECTOR('',#15496,1.);
#4306=VECTOR('',#15497,1.);
#4307=VECTOR('',#15500,1.);
#4308=VECTOR('',#15501,1.);
#4309=VECTOR('',#15502,1.);
#4310=VECTOR('',#15505,1.);
#4311=VECTOR('',#15506,1.);
#4312=VECTOR('',#15515,1.);
#4313=VECTOR('',#15524,1.);
#4314=VECTOR('',#15527,1.);
#4315=VECTOR('',#15528,0.475000000000001);
#4316=VECTOR('',#15533,1.);
#4317=VECTOR('',#15542,1.);
#4318=VECTOR('',#15545,1.);
#4319=VECTOR('',#15546,0.475000000000001);
#4320=VECTOR('',#15551,1.);
#4321=VECTOR('',#15552,1.);
#4322=VECTOR('',#15553,1.);
#4323=VECTOR('',#15554,1.);
#4324=VECTOR('',#15555,1.);
#4325=VECTOR('',#15558,1.);
#4326=VECTOR('',#15559,1.);
#4327=VECTOR('',#15560,1.);
#4328=VECTOR('',#15561,1.);
#4329=VECTOR('',#15562,1.);
#4330=VECTOR('',#15567,0.274999999999999);
#4331=VECTOR('',#15572,0.274999999999999);
#4332=VECTOR('',#15575,1.);
#4333=VECTOR('',#15576,1.);
#4334=VECTOR('',#15579,1.);
#4335=VECTOR('',#15580,1.);
#4336=VECTOR('',#15581,1.);
#4337=VECTOR('',#15582,1.);
#4338=VECTOR('',#15583,1.);
#4339=VECTOR('',#15586,1.);
#4340=VECTOR('',#15587,1.);
#4341=VECTOR('',#15590,1.);
#4342=VECTOR('',#15591,1.);
#4343=VECTOR('',#15594,1.);
#4344=VECTOR('',#15595,1.);
#4345=VECTOR('',#15596,1.);
#4346=VECTOR('',#15599,1.);
#4347=VECTOR('',#15600,1.);
#4348=VECTOR('',#15611,0.375);
#4349=VECTOR('',#15622,0.375);
#4350=VECTOR('',#15633,0.375);
#4351=VECTOR('',#15644,0.375);
#4352=VECTOR('',#15655,0.225);
#4353=VECTOR('',#15660,0.225);
#4354=VECTOR('',#15665,0.225);
#4355=VECTOR('',#15670,0.225000000000001);
#4356=VECTOR('',#15673,1.);
#4357=VECTOR('',#15674,1.);
#4358=VECTOR('',#15675,1.);
#4359=VECTOR('',#15676,1.);
#4360=VECTOR('',#15679,1.);
#4361=VECTOR('',#15680,1.);
#4362=VECTOR('',#15681,1.);
#4363=VECTOR('',#15684,1.);
#4364=VECTOR('',#15685,1.);
#4365=VECTOR('',#15686,1.);
#4366=VECTOR('',#15689,1.);
#4367=VECTOR('',#15690,1.);
#4368=VECTOR('',#15691,1.);
#4369=VECTOR('',#15694,1.);
#4370=VECTOR('',#15695,1.);
#4371=VECTOR('',#15696,1.);
#4372=VECTOR('',#15699,1.);
#4373=VECTOR('',#15700,1.);
#4374=VECTOR('',#15701,1.);
#4375=VECTOR('',#15704,1.);
#4376=VECTOR('',#15705,1.);
#4377=VECTOR('',#15706,1.);
#4378=VECTOR('',#15709,1.);
#4379=VECTOR('',#15710,1.);
#4380=VECTOR('',#15711,1.);
#4381=VECTOR('',#15714,1.);
#4382=VECTOR('',#15715,1.);
#4383=VECTOR('',#15716,1.);
#4384=VECTOR('',#15719,1.);
#4385=VECTOR('',#15720,1.);
#4386=VECTOR('',#15721,1.);
#4387=VECTOR('',#15724,1.);
#4388=VECTOR('',#15725,1.);
#4389=VECTOR('',#15726,1.);
#4390=VECTOR('',#15729,1.);
#4391=VECTOR('',#15730,1.);
#4392=VECTOR('',#15753,1.070235);
#4393=VECTOR('',#15760,0.6);
#4394=VECTOR('',#15765,0.63);
#4395=VECTOR('',#15774,1.070235);
#4396=VECTOR('',#15781,0.63);
#4397=VECTOR('',#15800,1.129765);
#4398=VECTOR('',#15811,1.57);
#4399=VECTOR('',#15816,1.6);
#4400=VECTOR('',#15821,1.57);
#4401=VECTOR('',#15826,1.129765);
#4402=VECTOR('',#15873,1.123812);
#4403=VECTOR('',#15942,1.076188);
#4404=VECTOR('',#15971,1.119765);
#4405=VECTOR('',#15978,1.085235);
#4406=VECTOR('',#15989,1.119765);
#4407=VECTOR('',#15996,1.085235);
#4408=VECTOR('',#16025,1.63531);
#4409=VECTOR('',#16032,1.);
#4410=VECTOR('',#16037,1.05);
#4411=VECTOR('',#16046,1.63531);
#4412=VECTOR('',#16053,1.05);
#4413=VECTOR('',#16072,1.71469);
#4414=VECTOR('',#16083,2.3);
#4415=VECTOR('',#16088,2.35);
#4416=VECTOR('',#16093,2.3);
#4417=VECTOR('',#16098,1.71469);
#4418=VECTOR('',#16149,1.706752);
#4419=VECTOR('',#16226,1.643248);
#4420=VECTOR('',#16255,1.70469);
#4421=VECTOR('',#16262,1.65031);
#4422=VECTOR('',#16273,1.70469);
#4423=VECTOR('',#16280,1.65031);
#4424=VECTOR('',#16295,1.);
#4425=VECTOR('',#16296,1.);
#4426=VECTOR('',#16297,1.);
#4427=VECTOR('',#16298,1.);
#4428=VECTOR('',#16301,1.);
#4429=VECTOR('',#16302,1.);
#4430=VECTOR('',#16303,1.);
#4431=VECTOR('',#16306,1.);
#4432=VECTOR('',#16307,1.);
#4433=VECTOR('',#16308,1.);
#4434=VECTOR('',#16311,1.);
#4435=VECTOR('',#16312,1.);
#4436=VECTOR('',#16313,1.);
#4437=VECTOR('',#16316,1.);
#4438=VECTOR('',#16317,1.);
#4439=VECTOR('',#16318,1.);
#4440=VECTOR('',#16321,1.);
#4441=VECTOR('',#16322,1.);
#4442=VECTOR('',#16323,1.);
#4443=VECTOR('',#16326,1.);
#4444=VECTOR('',#16327,1.);
#4445=VECTOR('',#16328,1.);
#4446=VECTOR('',#16331,1.);
#4447=VECTOR('',#16332,1.);
#4448=VECTOR('',#16333,1.);
#4449=VECTOR('',#16336,1.);
#4450=VECTOR('',#16337,1.);
#4451=VECTOR('',#16338,1.);
#4452=VECTOR('',#16341,1.);
#4453=VECTOR('',#16342,1.);
#4454=VECTOR('',#16343,1.);
#4455=VECTOR('',#16344,1.);
#4456=VECTOR('',#16347,1.);
#4457=VECTOR('',#16348,1.);
#4458=VECTOR('',#16349,1.);
#4459=VECTOR('',#16352,1.);
#4460=VECTOR('',#16353,1.);
#4461=VECTOR('',#16354,1.);
#4462=VECTOR('',#16357,1.);
#4463=VECTOR('',#16358,1.);
#4464=VECTOR('',#16359,1.);
#4465=VECTOR('',#16362,1.);
#4466=VECTOR('',#16363,1.);
#4467=VECTOR('',#16364,1.);
#4468=VECTOR('',#16367,1.);
#4469=VECTOR('',#16368,1.);
#4470=VECTOR('',#16369,1.);
#4471=VECTOR('',#16372,1.);
#4472=VECTOR('',#16373,1.);
#4473=VECTOR('',#16374,1.);
#4474=VECTOR('',#16377,1.);
#4475=VECTOR('',#16378,1.);
#4476=VECTOR('',#16379,1.);
#4477=VECTOR('',#16382,1.);
#4478=VECTOR('',#16383,1.);
#4479=VECTOR('',#16384,1.);
#4480=VECTOR('',#16387,1.);
#4481=VECTOR('',#16388,1.);
#4482=VECTOR('',#16389,1.);
#4483=VECTOR('',#16390,1.);
#4484=VECTOR('',#16393,1.);
#4485=VECTOR('',#16394,1.);
#4486=VECTOR('',#16395,1.);
#4487=VECTOR('',#16398,1.);
#4488=VECTOR('',#16399,1.);
#4489=VECTOR('',#16400,1.);
#4490=VECTOR('',#16403,1.);
#4491=VECTOR('',#16404,1.);
#4492=VECTOR('',#16405,1.);
#4493=VECTOR('',#16408,1.);
#4494=VECTOR('',#16409,1.);
#4495=VECTOR('',#16410,1.);
#4496=VECTOR('',#16413,1.);
#4497=VECTOR('',#16414,1.);
#4498=VECTOR('',#16415,1.);
#4499=VECTOR('',#16418,1.);
#4500=VECTOR('',#16419,1.);
#4501=VECTOR('',#16420,1.);
#4502=VECTOR('',#16423,1.);
#4503=VECTOR('',#16424,1.);
#4504=VECTOR('',#16425,1.);
#4505=VECTOR('',#16428,1.);
#4506=VECTOR('',#16429,1.);
#4507=VECTOR('',#16430,1.);
#4508=VECTOR('',#16433,1.);
#4509=VECTOR('',#16434,1.);
#4510=VECTOR('',#16435,1.);
#4511=VECTOR('',#16436,1.);
#4512=VECTOR('',#16439,1.);
#4513=VECTOR('',#16440,1.);
#4514=VECTOR('',#16441,1.);
#4515=VECTOR('',#16444,1.);
#4516=VECTOR('',#16445,1.);
#4517=VECTOR('',#16446,1.);
#4518=VECTOR('',#16449,1.);
#4519=VECTOR('',#16450,1.);
#4520=VECTOR('',#16451,1.);
#4521=VECTOR('',#16454,1.);
#4522=VECTOR('',#16455,1.);
#4523=VECTOR('',#16456,1.);
#4524=VECTOR('',#16459,1.);
#4525=VECTOR('',#16460,1.);
#4526=VECTOR('',#16461,1.);
#4527=VECTOR('',#16464,1.);
#4528=VECTOR('',#16465,1.);
#4529=VECTOR('',#16466,1.);
#4530=VECTOR('',#16469,1.);
#4531=VECTOR('',#16470,1.);
#4532=VECTOR('',#16471,1.);
#4533=VECTOR('',#16474,1.);
#4534=VECTOR('',#16475,1.);
#4535=VECTOR('',#16476,1.);
#4536=VECTOR('',#16481,0.21);
#4537=VECTOR('',#16486,1.);
#4538=VECTOR('',#16487,1.);
#4539=VECTOR('',#16488,1.);
#4540=VECTOR('',#16491,1.);
#4541=VECTOR('',#16492,1.);
#4542=VECTOR('',#16493,1.);
#4543=VECTOR('',#16496,1.);
#4544=VECTOR('',#16497,1.);
#4545=VECTOR('',#16500,1.);
#4546=VECTOR('',#16501,1.);
#4547=VECTOR('',#16502,1.);
#4548=VECTOR('',#16505,1.);
#4549=VECTOR('',#16506,1.);
#4550=VECTOR('',#16509,1.);
#4551=VECTOR('',#16510,1.);
#4552=VECTOR('',#16511,1.);
#4553=VECTOR('',#16514,1.);
#4554=VECTOR('',#16515,1.);
#4555=VECTOR('',#16518,1.);
#4556=VECTOR('',#16519,1.);
#4557=VECTOR('',#16528,1.);
#4558=VECTOR('',#16529,1.);
#4559=VECTOR('',#16530,1.);
#4560=VECTOR('',#16531,1.);
#4561=VECTOR('',#16534,1.);
#4562=VECTOR('',#16539,0.21);
#4563=VECTOR('',#16550,1.);
#4564=VECTOR('',#16551,1.);
#4565=VECTOR('',#16554,1.);
#4566=VECTOR('',#16555,1.);
#4567=VECTOR('',#16558,1.);
#4568=VECTOR('',#16559,1.);
#4569=VECTOR('',#16560,1.);
#4570=VECTOR('',#16563,1.);
#4571=VECTOR('',#16564,1.);
#4572=VECTOR('',#16565,1.);
#4573=VECTOR('',#16568,1.);
#4574=VECTOR('',#16569,1.);
#4575=VECTOR('',#16572,1.);
#4576=VECTOR('',#16573,1.);
#4577=VECTOR('',#16576,1.);
#4578=VECTOR('',#16585,0.275);
#4579=VECTOR('',#16590,0.265);
#4580=VECTOR('',#16599,0.5);
#4581=VECTOR('',#16608,1.);
#4582=VECTOR('',#16609,1.);
#4583=VECTOR('',#16610,1.);
#4584=VECTOR('',#16611,1.);
#4585=VECTOR('',#16614,1.);
#4586=VECTOR('',#16615,1.);
#4587=VECTOR('',#16616,1.);
#4588=VECTOR('',#16619,1.);
#4589=VECTOR('',#16620,1.);
#4590=VECTOR('',#16621,1.);
#4591=VECTOR('',#16624,1.);
#4592=VECTOR('',#16625,1.);
#4593=VECTOR('',#16626,1.);
#4594=VECTOR('',#16629,1.);
#4595=VECTOR('',#16630,1.);
#4596=VECTOR('',#16631,1.);
#4597=VECTOR('',#16634,1.);
#4598=VECTOR('',#16635,1.);
#4599=VECTOR('',#16652,0.4);
#4600=VECTOR('',#16657,0.425);
#4601=VECTOR('',#16662,0.41);
#4602=VECTOR('',#16671,0.26);
#4603=VECTOR('',#16674,0.25);
#4604=VECTOR('',#16683,0.275);
#4605=VECTOR('',#16690,0.275);
#4606=VECTOR('',#16697,0.275);
#4607=VECTOR('',#16704,0.275);
#4608=VECTOR('',#16709,1.);
#4609=VECTOR('',#16710,1.);
#4610=VECTOR('',#16711,1.);
#4611=VECTOR('',#16712,1.);
#4612=VECTOR('',#16715,1.);
#4613=VECTOR('',#16716,1.);
#4614=VECTOR('',#16717,1.);
#4615=VECTOR('',#16720,1.);
#4616=VECTOR('',#16721,1.);
#4617=VECTOR('',#16722,1.);
#4618=VECTOR('',#16725,1.);
#4619=VECTOR('',#16726,1.);
#4620=VECTOR('',#16737,0.275);
#4621=VECTOR('',#16744,0.275);
#4622=VECTOR('',#16751,0.275);
#4623=VECTOR('',#16758,0.275);
#4624=VECTOR('',#16765,0.275);
#4625=VECTOR('',#16772,0.275);
#4626=VECTOR('',#16779,0.275);
#4627=VECTOR('',#16786,0.275);
#4628=VECTOR('',#16791,1.);
#4629=VECTOR('',#16792,1.);
#4630=VECTOR('',#16793,1.);
#4631=VECTOR('',#16794,1.);
#4632=VECTOR('',#16797,1.);
#4633=VECTOR('',#16798,1.);
#4634=VECTOR('',#16799,1.);
#4635=VECTOR('',#16802,1.);
#4636=VECTOR('',#16803,1.);
#4637=VECTOR('',#16804,1.);
#4638=VECTOR('',#16807,1.);
#4639=VECTOR('',#16808,1.);
#4640=VECTOR('',#16819,0.210000000000001);
#4641=VECTOR('',#16828,0.210000000000001);
#4642=VECTOR('',#16837,0.210000000000001);
#4643=VECTOR('',#16846,0.210000000000001);
#4644=VECTOR('',#16855,0.165);
#4645=VECTOR('',#16864,0.165);
#4646=VECTOR('',#16873,0.165);
#4647=VECTOR('',#16882,1.11);
#4648=VECTOR('',#16887,1.);
#4649=VECTOR('',#16888,1.);
#4650=VECTOR('',#16889,1.);
#4651=VECTOR('',#16890,1.);
#4652=VECTOR('',#16893,1.);
#4653=VECTOR('',#16894,1.);
#4654=VECTOR('',#16895,1.);
#4655=VECTOR('',#16898,1.);
#4656=VECTOR('',#16899,1.);
#4657=VECTOR('',#16900,1.);
#4658=VECTOR('',#16903,1.);
#4659=VECTOR('',#16904,1.);
#4660=VECTOR('',#16915,1.);
#4661=VECTOR('',#16920,1.);
#4662=VECTOR('',#16923,0.21);
#4663=VECTOR('',#16928,1.);
#4664=VECTOR('',#16931,1.);
#4665=VECTOR('',#16936,1.);
#4666=VECTOR('',#16939,0.21);
#4667=VECTOR('',#16944,1.);
#4668=VECTOR('',#16947,1.);
#4669=VECTOR('',#16952,1.);
#4670=VECTOR('',#16955,0.21);
#4671=VECTOR('',#16960,1.);
#4672=VECTOR('',#16963,1.);
#4673=VECTOR('',#16968,1.);
#4674=VECTOR('',#16971,0.21);
#4675=VECTOR('',#16976,1.);
#4676=VECTOR('',#16979,1.);
#4677=VECTOR('',#16980,1.);
#4678=VECTOR('',#16981,1.);
#4679=VECTOR('',#16982,1.);
#4680=VECTOR('',#16983,1.);
#4681=VECTOR('',#16984,1.);
#4682=VECTOR('',#16987,1.);
#4683=VECTOR('',#16988,1.);
#4684=VECTOR('',#16989,1.);
#4685=VECTOR('',#16990,1.);
#4686=VECTOR('',#16991,1.);
#4687=VECTOR('',#16992,1.);
#4688=VECTOR('',#16995,1.);
#4689=VECTOR('',#16996,1.);
#4690=VECTOR('',#16997,1.);
#4691=VECTOR('',#16998,1.);
#4692=VECTOR('',#16999,1.);
#4693=VECTOR('',#17000,1.);
#4694=VECTOR('',#17001,1.);
#4695=VECTOR('',#17002,1.);
#4696=VECTOR('',#17003,1.);
#4697=VECTOR('',#17004,1.);
#4698=VECTOR('',#17007,1.);
#4699=VECTOR('',#17008,1.);
#4700=VECTOR('',#17011,1.);
#4701=VECTOR('',#17012,1.);
#4702=VECTOR('',#17015,1.);
#4703=VECTOR('',#17016,1.);
#4704=VECTOR('',#17019,1.);
#4705=VECTOR('',#17020,1.);
#4706=VECTOR('',#17023,1.);
#4707=VECTOR('',#17026,1.);
#4708=VECTOR('',#17027,1.);
#4709=VECTOR('',#17030,1.);
#4710=VECTOR('',#17031,1.);
#4711=VECTOR('',#17034,1.);
#4712=VECTOR('',#17035,1.);
#4713=VECTOR('',#17038,1.);
#4714=VECTOR('',#17039,1.);
#4715=VECTOR('',#17042,1.);
#4716=VECTOR('',#17049,1.);
#4717=VECTOR('',#17050,1.);
#4718=VECTOR('',#17051,1.);
#4719=VECTOR('',#17052,1.);
#4720=VECTOR('',#17055,1.);
#4721=VECTOR('',#17056,1.);
#4722=VECTOR('',#17057,1.);
#4723=VECTOR('',#17060,1.);
#4724=VECTOR('',#17061,1.);
#4725=VECTOR('',#17062,1.);
#4726=VECTOR('',#17065,1.);
#4727=VECTOR('',#17066,1.);
#4728=VECTOR('',#17067,1.);
#4729=VECTOR('',#17070,1.);
#4730=VECTOR('',#17071,1.);
#4731=VECTOR('',#17072,1.);
#4732=VECTOR('',#17075,1.);
#4733=VECTOR('',#17076,1.);
#4734=VECTOR('',#17077,1.);
#4735=VECTOR('',#17080,1.);
#4736=VECTOR('',#17081,1.);
#4737=VECTOR('',#17082,1.);
#4738=VECTOR('',#17085,1.);
#4739=VECTOR('',#17086,1.);
#4740=VECTOR('',#17095,1.);
#4741=VECTOR('',#17096,1.);
#4742=VECTOR('',#17097,1.);
#4743=VECTOR('',#17098,1.);
#4744=VECTOR('',#17101,1.);
#4745=VECTOR('',#17102,1.);
#4746=VECTOR('',#17103,1.);
#4747=VECTOR('',#17106,1.);
#4748=VECTOR('',#17107,1.);
#4749=VECTOR('',#17108,1.);
#4750=VECTOR('',#17111,1.);
#4751=VECTOR('',#17112,1.);
#4752=VECTOR('',#17113,1.);
#4753=VECTOR('',#17116,1.);
#4754=VECTOR('',#17117,1.);
#4755=VECTOR('',#17118,1.);
#4756=VECTOR('',#17121,1.);
#4757=VECTOR('',#17122,1.);
#4758=VECTOR('',#17123,1.);
#4759=VECTOR('',#17126,1.);
#4760=VECTOR('',#17127,1.);
#4761=VECTOR('',#17128,1.);
#4762=VECTOR('',#17131,1.);
#4763=VECTOR('',#17132,1.);
#4764=VECTOR('',#17149,0.275);
#4765=VECTOR('',#17154,0.265);
#4766=VECTOR('',#17163,0.5);
#4767=VECTOR('',#17172,1.);
#4768=VECTOR('',#17173,1.);
#4769=VECTOR('',#17174,1.);
#4770=VECTOR('',#17175,1.);
#4771=VECTOR('',#17178,1.);
#4772=VECTOR('',#17179,1.);
#4773=VECTOR('',#17180,1.);
#4774=VECTOR('',#17183,1.);
#4775=VECTOR('',#17184,1.);
#4776=VECTOR('',#17185,1.);
#4777=VECTOR('',#17188,1.);
#4778=VECTOR('',#17189,1.);
#4779=VECTOR('',#17190,1.);
#4780=VECTOR('',#17193,1.);
#4781=VECTOR('',#17194,1.);
#4782=VECTOR('',#17195,1.);
#4783=VECTOR('',#17198,1.);
#4784=VECTOR('',#17199,1.);
#4785=VECTOR('',#17212,0.25);
#4786=VECTOR('',#17225,0.4);
#4787=VECTOR('',#17230,0.425);
#4788=VECTOR('',#17235,0.41);
#4789=VECTOR('',#17244,0.26);
#4790=VECTOR('',#17247,0.25);
#4791=VECTOR('',#17252,0.45);
#4792=VECTOR('',#17257,0.45);
#4793=VECTOR('',#17260,0.45);
#4794=VECTOR('',#17263,0.45);
#4795=VECTOR('',#17266,0.45);
#4796=VECTOR('',#17269,0.45);
#4797=VECTOR('',#17272,0.45);
#4798=VECTOR('',#17275,0.45);
#4799=VECTOR('',#17278,0.45);
#4800=VECTOR('',#17283,0.625);
#4801=VECTOR('',#17288,0.625);
#4802=VECTOR('',#17291,0.625);
#4803=VECTOR('',#17294,0.625);
#4804=VECTOR('',#17297,0.625);
#4805=VECTOR('',#17300,0.625);
#4806=VECTOR('',#17303,0.625);
#4807=VECTOR('',#17306,0.625);
#4808=VECTOR('',#17309,0.625);
#4809=VECTOR('',#17316,1.);
#4810=VECTOR('',#17331,0.225);
#4811=VECTOR('',#17336,0.225);
#4812=VECTOR('',#17341,0.225);
#4813=VECTOR('',#17344,1.);
#4814=VECTOR('',#17345,1.);
#4815=VECTOR('',#17346,1.);
#4816=VECTOR('',#17359,1.1);
#4817=VECTOR('',#17374,0.325);
#4818=VECTOR('',#17379,0.35);
#4819=VECTOR('',#17384,0.335);
#4820=VECTOR('',#17393,0.21);
#4821=VECTOR('',#17398,0.2);
#4822=VECTOR('',#17403,0.18);
#4823=VECTOR('',#17408,1.);
#4824=VECTOR('',#17409,1.);
#4825=VECTOR('',#17410,1.);
#4826=VECTOR('',#17411,1.);
#4827=VECTOR('',#17414,1.);
#4828=VECTOR('',#17415,1.);
#4829=VECTOR('',#17416,1.);
#4830=VECTOR('',#17419,1.);
#4831=VECTOR('',#17420,1.);
#4832=VECTOR('',#17421,1.);
#4833=VECTOR('',#17424,1.);
#4834=VECTOR('',#17425,1.);
#4835=VECTOR('',#17426,1.);
#4836=VECTOR('',#17429,1.);
#4837=VECTOR('',#17430,1.);
#4838=VECTOR('',#17431,1.);
#4839=VECTOR('',#17434,1.);
#4840=VECTOR('',#17435,1.);
#4841=VECTOR('',#17450,0.4);
#4842=VECTOR('',#17455,0.425);
#4843=VECTOR('',#17460,0.41);
#4844=VECTOR('',#17469,0.26);
#4845=VECTOR('',#17474,0.25);
#4846=VECTOR('',#17479,0.225);
#4847=VECTOR('',#17484,1.);
#4848=VECTOR('',#17485,1.);
#4849=VECTOR('',#17486,1.);
#4850=VECTOR('',#17487,1.);
#4851=VECTOR('',#17490,1.);
#4852=VECTOR('',#17491,1.);
#4853=VECTOR('',#17492,1.);
#4854=VECTOR('',#17495,1.);
#4855=VECTOR('',#17496,1.);
#4856=VECTOR('',#17497,1.);
#4857=VECTOR('',#17500,1.);
#4858=VECTOR('',#17501,1.);
#4859=VECTOR('',#17502,1.);
#4860=VECTOR('',#17505,1.);
#4861=VECTOR('',#17506,1.);
#4862=VECTOR('',#17507,1.);
#4863=VECTOR('',#17510,1.);
#4864=VECTOR('',#17511,1.);
#4865=VECTOR('',#17562,0.6);
#4866=VECTOR('',#17567,0.6);
#4867=VECTOR('',#17570,0.6);
#4868=VECTOR('',#17573,0.6);
#4869=VECTOR('',#17576,0.6);
#4870=VECTOR('',#17579,0.6);
#4871=VECTOR('',#17582,0.6);
#4872=VECTOR('',#17585,0.6);
#4873=VECTOR('',#17588,0.6);
#4874=VECTOR('',#17591,0.6);
#4875=VECTOR('',#17594,0.6);
#4876=VECTOR('',#17597,0.6);
#4877=VECTOR('',#17600,0.6);
#4878=VECTOR('',#17603,0.6);
#4879=VECTOR('',#17606,0.6);
#4880=VECTOR('',#17609,0.6);
#4881=VECTOR('',#17612,0.6);
#4882=VECTOR('',#17615,0.6);
#4883=VECTOR('',#17618,0.6);
#4884=VECTOR('',#17621,0.6);
#4885=VECTOR('',#17624,0.6);
#4886=VECTOR('',#17627,0.6);
#4887=VECTOR('',#17630,0.6);
#4888=VECTOR('',#17633,0.6);
#4889=VECTOR('',#17636,0.6);
#4890=VECTOR('',#17639,0.6);
#4891=VECTOR('',#17642,0.6);
#4892=VECTOR('',#17645,0.6);
#4893=VECTOR('',#17648,0.6);
#4894=VECTOR('',#17651,0.6);
#4895=VECTOR('',#17654,0.6);
#4896=VECTOR('',#17657,0.6);
#4897=VECTOR('',#17660,0.6);
#4898=VECTOR('',#17663,0.6);
#4899=VECTOR('',#17666,0.6);
#4900=VECTOR('',#17669,0.6);
#4901=VECTOR('',#17672,0.6);
#4902=VECTOR('',#17675,0.6);
#4903=VECTOR('',#17678,0.6);
#4904=VECTOR('',#17681,0.6);
#4905=VECTOR('',#17684,0.6);
#4906=VECTOR('',#17687,0.6);
#4907=VECTOR('',#17690,0.6);
#4908=VECTOR('',#17693,0.6);
#4909=VECTOR('',#17696,0.6);
#4910=VECTOR('',#17699,0.6);
#4911=VECTOR('',#17702,0.6);
#4912=VECTOR('',#17705,0.6);
#4913=VECTOR('',#17708,0.6);
#4914=VECTOR('',#17711,0.6);
#4915=VECTOR('',#17714,0.6);
#4916=VECTOR('',#17717,0.6);
#4917=VECTOR('',#17720,0.6);
#4918=VECTOR('',#17723,0.6);
#4919=VECTOR('',#17726,0.6);
#4920=VECTOR('',#17729,0.6);
#4921=VECTOR('',#17732,0.6);
#4922=VECTOR('',#17735,0.6);
#4923=VECTOR('',#17738,0.6);
#4924=VECTOR('',#17741,0.6);
#4925=VECTOR('',#17744,0.6);
#4926=VECTOR('',#17747,0.6);
#4927=VECTOR('',#17750,0.6);
#4928=VECTOR('',#17753,0.415875);
#4929=VECTOR('',#17758,0.415875);
#4930=VECTOR('',#17763,0.415875);
#4931=VECTOR('',#17766,0.415875);
#4932=VECTOR('',#17769,0.415875);
#4933=VECTOR('',#17772,0.415875);
#4934=VECTOR('',#17775,0.415875);
#4935=VECTOR('',#17778,0.415875);
#4936=VECTOR('',#17781,0.415875);
#4937=VECTOR('',#17784,0.415875);
#4938=VECTOR('',#17787,0.415875);
#4939=VECTOR('',#17790,0.415875);
#4940=VECTOR('',#17793,0.415875);
#4941=VECTOR('',#17796,0.415875);
#4942=VECTOR('',#17799,0.415875);
#4943=VECTOR('',#17802,0.415875);
#4944=VECTOR('',#17805,0.415875);
#4945=VECTOR('',#17808,0.415875);
#4946=VECTOR('',#17811,0.415875);
#4947=VECTOR('',#17814,0.415875);
#4948=VECTOR('',#17817,0.415875);
#4949=VECTOR('',#17820,0.415875);
#4950=VECTOR('',#17823,0.415875);
#4951=VECTOR('',#17826,0.415875);
#4952=VECTOR('',#17829,0.415875);
#4953=VECTOR('',#17832,0.415875);
#4954=VECTOR('',#17835,0.415875);
#4955=VECTOR('',#17838,0.415875);
#4956=VECTOR('',#17841,0.415875);
#4957=VECTOR('',#17844,0.415875);
#4958=VECTOR('',#17847,0.415875);
#4959=VECTOR('',#17850,0.415875);
#4960=VECTOR('',#17853,0.415875);
#4961=VECTOR('',#17856,0.415875);
#4962=VECTOR('',#17859,0.415875);
#4963=VECTOR('',#17862,0.415875);
#4964=VECTOR('',#17865,0.415875);
#4965=VECTOR('',#17868,0.415875);
#4966=VECTOR('',#17871,0.415875);
#4967=VECTOR('',#17874,0.415875);
#4968=VECTOR('',#17877,0.415875);
#4969=VECTOR('',#17880,0.415875);
#4970=VECTOR('',#17883,0.415875);
#4971=VECTOR('',#17886,0.415875);
#4972=VECTOR('',#17889,0.415875);
#4973=VECTOR('',#17892,0.415875);
#4974=VECTOR('',#17895,0.415875);
#4975=VECTOR('',#17898,0.415875);
#4976=VECTOR('',#17901,0.415875);
#4977=VECTOR('',#17904,0.415875);
#4978=VECTOR('',#17907,0.415875);
#4979=VECTOR('',#17910,0.415875);
#4980=VECTOR('',#17913,0.415875);
#4981=VECTOR('',#17916,0.415875);
#4982=VECTOR('',#17919,0.415875);
#4983=VECTOR('',#17922,0.415875);
#4984=VECTOR('',#17925,0.415875);
#4985=VECTOR('',#17928,0.415875);
#4986=VECTOR('',#17931,0.415875);
#4987=VECTOR('',#17934,0.415875);
#4988=VECTOR('',#17937,0.415875);
#4989=VECTOR('',#17940,0.415875);
#4990=VECTOR('',#17943,0.415875);
#4991=VECTOR('',#17952,0.6);
#4992=VECTOR('',#17961,1.);
#4993=VECTOR('',#17962,1.);
#4994=VECTOR('',#17963,1.);
#4995=VECTOR('',#17964,1.);
#4996=VECTOR('',#17969,1.);
#4997=VECTOR('',#17970,1.);
#4998=VECTOR('',#17973,1.);
#4999=VECTOR('',#17974,1.);
#5000=VECTOR('',#17977,1.);
#5001=VECTOR('',#17978,1.);
#5002=VECTOR('',#17987,1.);
#5003=VECTOR('',#18002,1.35);
#5004=VECTOR('',#18013,1.01);
#5005=VECTOR('',#18020,1.35);
#5006=VECTOR('',#18031,1.);
#5007=VECTOR('',#18038,0.210000000000001);
#5008=VECTOR('',#18041,1.);
#5009=VECTOR('',#18046,1.005);
#5010=VECTOR('',#18053,1.5);
#5011=VECTOR('',#18066,0.25);
#5012=VECTOR('',#18071,1.);
#5013=VECTOR('',#18078,0.210000000000001);
#5014=VECTOR('',#18081,1.);
#5015=VECTOR('',#18084,1.);
#5016=VECTOR('',#18085,1.);
#5017=VECTOR('',#18086,1.);
#5018=VECTOR('',#18087,1.);
#5019=VECTOR('',#18088,1.);
#5020=VECTOR('',#18089,1.);
#5021=VECTOR('',#18092,1.);
#5022=VECTOR('',#18093,1.);
#5023=VECTOR('',#18094,1.);
#5024=VECTOR('',#18097,1.);
#5025=VECTOR('',#18098,1.);
#5026=VECTOR('',#18099,1.);
#5027=VECTOR('',#18100,1.);
#5028=VECTOR('',#18101,1.);
#5029=VECTOR('',#18116,3.5);
#5030=VECTOR('',#18133,0.33);
#5031=VECTOR('',#18140,0.4);
#5032=VECTOR('',#18153,0.405);
#5033=VECTOR('',#18160,0.9);
#5034=VECTOR('',#18171,1.);
#5035=VECTOR('',#18172,1.);
#5036=VECTOR('',#18173,1.);
#5037=VECTOR('',#18174,1.);
#5038=VECTOR('',#18175,1.);
#5039=VECTOR('',#18176,1.);
#5040=VECTOR('',#18177,1.);
#5041=VECTOR('',#18178,1.);
#5042=VECTOR('',#18181,1.);
#5043=VECTOR('',#18182,1.);
#5044=VECTOR('',#18183,1.);
#5045=VECTOR('',#18186,1.);
#5046=VECTOR('',#18187,1.);
#5047=VECTOR('',#18190,1.);
#5048=VECTOR('',#18191,1.);
#5049=VECTOR('',#18194,1.);
#5050=VECTOR('',#18195,1.);
#5051=VECTOR('',#18198,1.);
#5052=VECTOR('',#18199,1.);
#5053=VECTOR('',#18200,1.);
#5054=VECTOR('',#18201,1.);
#5055=VECTOR('',#18204,1.);
#5056=VECTOR('',#18207,1.);
#5057=VECTOR('',#18210,1.);
#5058=VECTOR('',#18217,1.);
#5059=VECTOR('',#18218,1.);
#5060=VECTOR('',#18219,1.);
#5061=VECTOR('',#18220,1.);
#5062=VECTOR('',#18223,1.);
#5063=VECTOR('',#18224,1.);
#5064=VECTOR('',#18225,1.);
#5065=VECTOR('',#18228,1.);
#5066=VECTOR('',#18229,1.);
#5067=VECTOR('',#18230,1.);
#5068=VECTOR('',#18233,1.);
#5069=VECTOR('',#18234,1.);
#5070=VECTOR('',#18235,1.);
#5071=VECTOR('',#18238,1.);
#5072=VECTOR('',#18239,1.);
#5073=VECTOR('',#18240,1.);
#5074=VECTOR('',#18243,1.);
#5075=VECTOR('',#18244,1.);
#5076=VECTOR('',#18255,0.235);
#5077=VECTOR('',#18260,0.25);
#5078=VECTOR('',#18265,0.2125);
#5079=VECTOR('',#18274,0.32);
#5080=VECTOR('',#18281,0.6);
#5081=VECTOR('',#18298,0.475);
#5082=VECTOR('',#18303,0.5);
#5083=VECTOR('',#18308,0.485);
#5084=VECTOR('',#18317,0.31);
#5085=VECTOR('',#18322,0.3);
#5086=VECTOR('',#18327,0.27);
#5087=VECTOR('',#18332,1.);
#5088=VECTOR('',#18333,1.);
#5089=VECTOR('',#18334,1.);
#5090=VECTOR('',#18335,1.);
#5091=VECTOR('',#18338,1.);
#5092=VECTOR('',#18339,1.);
#5093=VECTOR('',#18340,1.);
#5094=VECTOR('',#18343,1.);
#5095=VECTOR('',#18344,1.);
#5096=VECTOR('',#18345,1.);
#5097=VECTOR('',#18348,1.);
#5098=VECTOR('',#18349,1.);
#5099=VECTOR('',#18350,1.);
#5100=VECTOR('',#18353,1.);
#5101=VECTOR('',#18354,1.);
#5102=VECTOR('',#18355,1.);
#5103=VECTOR('',#18358,1.);
#5104=VECTOR('',#18359,1.);
#5105=CIRCLE('',#13563,0.274999999999999);
#5106=CIRCLE('',#13564,0.274999999999999);
#5107=CIRCLE('',#13566,0.275);
#5108=CIRCLE('',#13567,0.275);
#5109=CIRCLE('',#13569,0.275);
#5110=CIRCLE('',#13570,0.275);
#5111=CIRCLE('',#13572,0.274999999999999);
#5112=CIRCLE('',#13573,0.274999999999999);
#5113=CIRCLE('',#13575,0.210000000000001);
#5114=CIRCLE('',#13576,0.210000000000001);
#5115=CIRCLE('',#13578,0.210000000000001);
#5116=CIRCLE('',#13579,0.210000000000001);
#5117=CIRCLE('',#13581,0.21);
#5118=CIRCLE('',#13582,0.21);
#5119=CIRCLE('',#13584,0.21);
#5120=CIRCLE('',#13585,0.21);
#5121=CIRCLE('',#13587,0.329999999999998);
#5122=CIRCLE('',#13588,0.329999999999998);
#5123=CIRCLE('',#13590,0.329999999999998);
#5124=CIRCLE('',#13591,0.329999999999998);
#5125=CIRCLE('',#13593,0.275);
#5126=CIRCLE('',#13594,0.275);
#5127=CIRCLE('',#13596,0.275);
#5128=CIRCLE('',#13597,0.275);
#5129=CIRCLE('',#13599,0.210000000000001);
#5130=CIRCLE('',#13600,0.210000000000001);
#5131=CIRCLE('',#13602,0.21);
#5132=CIRCLE('',#13603,0.21);
#5133=CIRCLE('',#13605,0.21);
#5134=CIRCLE('',#13606,0.21);
#5135=CIRCLE('',#13608,0.210000000000001);
#5136=CIRCLE('',#13609,0.210000000000001);
#5137=CIRCLE('',#13618,0.164999999999999);
#5138=CIRCLE('',#13619,0.164999999999999);
#5139=CIRCLE('',#13621,0.164999999999999);
#5140=CIRCLE('',#13622,0.164999999999999);
#5141=CIRCLE('',#13624,0.165);
#5142=CIRCLE('',#13625,0.165);
#5143=CIRCLE('',#13627,0.164999999999999);
#5144=CIRCLE('',#13628,0.164999999999999);
#5145=CIRCLE('',#13630,0.5);
#5146=CIRCLE('',#13631,0.5);
#5147=CIRCLE('',#13633,0.274999999999999);
#5148=CIRCLE('',#13635,0.5);
#5149=CIRCLE('',#13636,0.5);
#5150=CIRCLE('',#13638,0.275);
#5151=CIRCLE('',#13640,0.5);
#5152=CIRCLE('',#13641,0.5);
#5153=CIRCLE('',#13643,0.275);
#5154=CIRCLE('',#13645,0.5);
#5155=CIRCLE('',#13646,0.5);
#5156=CIRCLE('',#13648,0.274999999999999);
#5157=CIRCLE('',#13650,0.274999999999999);
#5158=CIRCLE('',#13652,0.275);
#5159=CIRCLE('',#13654,0.275);
#5160=CIRCLE('',#13656,0.274999999999999);
#5161=CIRCLE('',#13665,0.165);
#5162=CIRCLE('',#13666,0.165);
#5163=CIRCLE('',#13668,0.165);
#5164=CIRCLE('',#13669,0.165);
#5165=CIRCLE('',#13671,0.165);
#5166=CIRCLE('',#13672,0.165);
#5167=CIRCLE('',#13674,1.6);
#5168=CIRCLE('',#13675,1.6);
#5169=CIRCLE('',#13677,1.4);
#5170=CIRCLE('',#13679,1.4);
#5171=CIRCLE('',#13681,0.21);
#5172=CIRCLE('',#13682,0.21);
#5173=CIRCLE('',#13685,0.21);
#5174=CIRCLE('',#13686,0.21);
#5175=CIRCLE('',#13696,0.225);
#5176=CIRCLE('',#13697,0.225);
#5177=CIRCLE('',#13699,0.225);
#5178=CIRCLE('',#13700,0.225);
#5179=CIRCLE('',#13702,0.225);
#5180=CIRCLE('',#13703,0.225);
#5181=CIRCLE('',#13705,1.59);
#5182=CIRCLE('',#13706,1.59);
#5183=CIRCLE('',#13708,1.2);
#5184=CIRCLE('',#13710,1.2);
#5185=CIRCLE('',#13712,2.4);
#5186=CIRCLE('',#13713,2.4);
#5187=CIRCLE('',#13718,0.165);
#5188=CIRCLE('',#13719,0.165);
#5189=CIRCLE('',#13721,0.165);
#5190=CIRCLE('',#13722,0.165);
#5191=CIRCLE('',#13724,0.165);
#5192=CIRCLE('',#13725,0.165);
#5193=CIRCLE('',#13727,2.35);
#5194=CIRCLE('',#13728,2.35);
#5195=CIRCLE('',#13730,2.15);
#5196=CIRCLE('',#13732,2.15);
#5197=CIRCLE('',#13734,0.25);
#5198=CIRCLE('',#13735,0.25);
#5199=CIRCLE('',#13738,0.25);
#5200=CIRCLE('',#13739,0.25);
#5201=CIRCLE('',#13750,3.);
#5202=CIRCLE('',#13751,2.34);
#5203=CIRCLE('',#13752,0.225);
#5204=CIRCLE('',#13753,0.225);
#5205=CIRCLE('',#13754,0.225);
#5206=CIRCLE('',#13756,3.);
#5207=CIRCLE('',#13758,0.225);
#5208=CIRCLE('',#13760,0.225);
#5209=CIRCLE('',#13762,0.225);
#5210=CIRCLE('',#13764,2.34);
#5211=CIRCLE('',#13766,1.8);
#5212=CIRCLE('',#13768,1.8);
#5213=CIRCLE('',#13772,0.475);
#5214=CIRCLE('',#13773,0.475);
#5215=CIRCLE('',#13774,0.275);
#5216=CIRCLE('',#13776,0.475);
#5217=CIRCLE('',#13777,0.475);
#5218=CIRCLE('',#13779,0.475);
#5219=CIRCLE('',#13780,0.475);
#5220=CIRCLE('',#13781,0.275);
#5221=CIRCLE('',#13783,0.475);
#5222=CIRCLE('',#13784,0.475);
#5223=CIRCLE('',#13788,0.275);
#5224=CIRCLE('',#13790,0.275);
#5225=CIRCLE('',#13801,0.475000000000001);
#5226=CIRCLE('',#13802,0.475000000000001);
#5227=CIRCLE('',#13803,0.274999999999999);
#5228=CIRCLE('',#13805,0.475000000000001);
#5229=CIRCLE('',#13806,0.475000000000001);
#5230=CIRCLE('',#13808,0.475000000000001);
#5231=CIRCLE('',#13809,0.475000000000001);
#5232=CIRCLE('',#13810,0.274999999999999);
#5233=CIRCLE('',#13812,0.475000000000001);
#5234=CIRCLE('',#13813,0.475000000000001);
#5235=CIRCLE('',#13817,0.274999999999999);
#5236=CIRCLE('',#13819,0.274999999999999);
#5237=CIRCLE('',#13830,0.375);
#5238=CIRCLE('',#13831,0.375);
#5239=CIRCLE('',#13833,0.225);
#5240=CIRCLE('',#13835,0.375);
#5241=CIRCLE('',#13836,0.375);
#5242=CIRCLE('',#13838,0.225);
#5243=CIRCLE('',#13840,0.375);
#5244=CIRCLE('',#13841,0.375);
#5245=CIRCLE('',#13843,0.225);
#5246=CIRCLE('',#13845,0.375);
#5247=CIRCLE('',#13846,0.375);
#5248=CIRCLE('',#13848,0.225000000000001);
#5249=CIRCLE('',#13850,0.225);
#5250=CIRCLE('',#13852,0.225);
#5251=CIRCLE('',#13854,0.225);
#5252=CIRCLE('',#13856,0.225000000000001);
#5253=CIRCLE('',#13874,1.070235);
#5254=CIRCLE('',#13875,1.070235);
#5255=CIRCLE('',#13876,0.309556);
#5256=CIRCLE('',#13877,1.070235);
#5257=CIRCLE('',#13878,1.070235);
#5258=CIRCLE('',#13880,1.070235);
#5259=CIRCLE('',#13882,0.6);
#5260=CIRCLE('',#13883,0.6);
#5261=CIRCLE('',#13885,0.66);
#5262=CIRCLE('',#13888,1.070235);
#5263=CIRCLE('',#13890,0.66);
#5264=CIRCLE('',#13894,1.129765);
#5265=CIRCLE('',#13895,1.129765);
#5266=CIRCLE('',#13896,0.309556);
#5267=CIRCLE('',#13897,1.129765);
#5268=CIRCLE('',#13898,1.129765);
#5269=CIRCLE('',#13900,1.129765);
#5270=CIRCLE('',#13902,1.54);
#5271=CIRCLE('',#13903,1.129765);
#5272=CIRCLE('',#13905,1.6);
#5273=CIRCLE('',#13907,1.6);
#5274=CIRCLE('',#13909,1.54);
#5275=CIRCLE('',#13914,0.29765);
#5276=CIRCLE('',#13916,0.29765);
#5277=CIRCLE('',#13918,0.29765);
#5278=CIRCLE('',#13920,0.29765);
#5279=CIRCLE('',#13922,0.29765);
#5280=CIRCLE('',#13924,0.29765);
#5281=CIRCLE('',#13926,0.29765);
#5282=CIRCLE('',#13929,0.303778037777585);
#5283=CIRCLE('',#13930,0.303778037777585);
#5284=CIRCLE('',#13932,1.123812);
#5285=CIRCLE('',#13933,1.123812);
#5286=CIRCLE('',#13934,1.123812);
#5287=CIRCLE('',#13935,1.123812);
#5288=CIRCLE('',#13936,1.123812);
#5289=CIRCLE('',#13937,1.123812);
#5290=CIRCLE('',#13938,1.123812);
#5291=CIRCLE('',#13939,1.123812);
#5292=CIRCLE('',#13940,1.123812);
#5293=CIRCLE('',#13942,1.076188);
#5294=CIRCLE('',#13943,0.303778037777585);
#5295=CIRCLE('',#13945,0.303778037777585);
#5296=CIRCLE('',#13947,1.076188);
#5297=CIRCLE('',#13948,0.303778037777585);
#5298=CIRCLE('',#13950,0.303778037777585);
#5299=CIRCLE('',#13952,1.076188);
#5300=CIRCLE('',#13953,1.076188);
#5301=CIRCLE('',#13954,0.303778037777585);
#5302=CIRCLE('',#13956,0.303778037777585);
#5303=CIRCLE('',#13958,1.076188);
#5304=CIRCLE('',#13959,0.303778037777585);
#5305=CIRCLE('',#13961,0.303778037777585);
#5306=CIRCLE('',#13963,1.076188);
#5307=CIRCLE('',#13964,0.303778037777585);
#5308=CIRCLE('',#13966,0.303778037777585);
#5309=CIRCLE('',#13968,1.076188);
#5310=CIRCLE('',#13969,1.076188);
#5311=CIRCLE('',#13970,1.076188);
#5312=CIRCLE('',#13972,0.303778037777585);
#5313=CIRCLE('',#13974,0.303778037777585);
#5314=CIRCLE('',#13979,1.119765);
#5315=CIRCLE('',#13980,1.085235);
#5316=CIRCLE('',#13982,1.119765);
#5317=CIRCLE('',#13984,1.085235);
#5318=CIRCLE('',#13987,1.119765);
#5319=CIRCLE('',#13988,1.085235);
#5320=CIRCLE('',#13990,1.119765);
#5321=CIRCLE('',#13992,1.085235);
#5322=CIRCLE('',#14002,1.63531);
#5323=CIRCLE('',#14003,1.63531);
#5324=CIRCLE('',#14004,0.412776);
#5325=CIRCLE('',#14005,1.63531);
#5326=CIRCLE('',#14006,1.63531);
#5327=CIRCLE('',#14008,1.63531);
#5328=CIRCLE('',#14010,1.);
#5329=CIRCLE('',#14011,1.);
#5330=CIRCLE('',#14013,1.1);
#5331=CIRCLE('',#14016,1.63531);
#5332=CIRCLE('',#14018,1.1);
#5333=CIRCLE('',#14022,1.71469);
#5334=CIRCLE('',#14023,1.71469);
#5335=CIRCLE('',#14024,0.412776);
#5336=CIRCLE('',#14025,1.71469);
#5337=CIRCLE('',#14026,1.71469);
#5338=CIRCLE('',#14028,1.71469);
#5339=CIRCLE('',#14030,2.25);
#5340=CIRCLE('',#14031,1.71469);
#5341=CIRCLE('',#14033,2.35);
#5342=CIRCLE('',#14035,2.35);
#5343=CIRCLE('',#14037,2.25);
#5344=CIRCLE('',#14042,0.3969);
#5345=CIRCLE('',#14044,0.3969);
#5346=CIRCLE('',#14046,0.3969);
#5347=CIRCLE('',#14048,0.3969);
#5348=CIRCLE('',#14050,0.3969);
#5349=CIRCLE('',#14052,0.3969);
#5350=CIRCLE('',#14054,0.3969);
#5351=CIRCLE('',#14056,0.3969);
#5352=CIRCLE('',#14059,0.405071403305639);
#5353=CIRCLE('',#14060,0.405071403305639);
#5354=CIRCLE('',#14062,1.706752);
#5355=CIRCLE('',#14063,1.706752);
#5356=CIRCLE('',#14064,1.706752);
#5357=CIRCLE('',#14065,1.706752);
#5358=CIRCLE('',#14066,1.706752);
#5359=CIRCLE('',#14067,1.706752);
#5360=CIRCLE('',#14068,1.706752);
#5361=CIRCLE('',#14069,1.706752);
#5362=CIRCLE('',#14070,1.706752);
#5363=CIRCLE('',#14072,1.643248);
#5364=CIRCLE('',#14073,0.405071403305639);
#5365=CIRCLE('',#14075,0.405071403305639);
#5366=CIRCLE('',#14077,1.643248);
#5367=CIRCLE('',#14078,0.405071403305639);
#5368=CIRCLE('',#14080,0.405071403305639);
#5369=CIRCLE('',#14082,1.643248);
#5370=CIRCLE('',#14083,0.405071403305639);
#5371=CIRCLE('',#14085,0.405071403305639);
#5372=CIRCLE('',#14087,1.643248);
#5373=CIRCLE('',#14088,0.405071403305639);
#5374=CIRCLE('',#14090,0.405071403305639);
#5375=CIRCLE('',#14092,1.643248);
#5376=CIRCLE('',#14093,0.405071403305639);
#5377=CIRCLE('',#14095,0.405071403305639);
#5378=CIRCLE('',#14097,1.643248);
#5379=CIRCLE('',#14098,0.405071403305639);
#5380=CIRCLE('',#14100,0.405071403305639);
#5381=CIRCLE('',#14102,1.643248);
#5382=CIRCLE('',#14103,1.643248);
#5383=CIRCLE('',#14104,1.643248);
#5384=CIRCLE('',#14106,0.405071403305639);
#5385=CIRCLE('',#14108,0.405071403305639);
#5386=CIRCLE('',#14113,1.70469);
#5387=CIRCLE('',#14114,1.65031);
#5388=CIRCLE('',#14116,1.70469);
#5389=CIRCLE('',#14118,1.65031);
#5390=CIRCLE('',#14121,1.70469);
#5391=CIRCLE('',#14122,1.65031);
#5392=CIRCLE('',#14124,1.70469);
#5393=CIRCLE('',#14126,1.65031);
#5394=CIRCLE('',#14171,0.21);
#5395=CIRCLE('',#14172,0.21);
#5396=CIRCLE('',#14187,0.2117);
#5397=CIRCLE('',#14188,0.2117);
#5398=CIRCLE('',#14189,0.2117);
#5399=CIRCLE('',#14191,0.2117);
#5400=CIRCLE('',#14202,0.285);
#5401=CIRCLE('',#14203,0.265);
#5402=CIRCLE('',#14205,0.265);
#5403=CIRCLE('',#14207,0.5);
#5404=CIRCLE('',#14209,0.5);
#5405=CIRCLE('',#14221,0.24505);
#5406=CIRCLE('',#14223,0.375);
#5407=CIRCLE('',#14225,0.425);
#5408=CIRCLE('',#14227,0.425);
#5409=CIRCLE('',#14229,0.395);
#5410=CIRCLE('',#14231,0.27);
#5411=CIRCLE('',#14233,0.24505);
#5412=CIRCLE('',#14238,0.275);
#5413=CIRCLE('',#14239,0.275);
#5414=CIRCLE('',#14241,0.275);
#5415=CIRCLE('',#14242,0.275);
#5416=CIRCLE('',#14244,0.275);
#5417=CIRCLE('',#14245,0.275);
#5418=CIRCLE('',#14247,0.275);
#5419=CIRCLE('',#14248,0.275);
#5420=CIRCLE('',#14257,0.275);
#5421=CIRCLE('',#14258,0.275);
#5422=CIRCLE('',#14260,0.275);
#5423=CIRCLE('',#14261,0.275);
#5424=CIRCLE('',#14263,0.275);
#5425=CIRCLE('',#14264,0.275);
#5426=CIRCLE('',#14266,0.275);
#5427=CIRCLE('',#14267,0.275);
#5428=CIRCLE('',#14269,0.275);
#5429=CIRCLE('',#14270,0.275);
#5430=CIRCLE('',#14272,0.275);
#5431=CIRCLE('',#14273,0.275);
#5432=CIRCLE('',#14275,0.275);
#5433=CIRCLE('',#14276,0.275);
#5434=CIRCLE('',#14278,0.275);
#5435=CIRCLE('',#14279,0.275);
#5436=CIRCLE('',#14288,0.210000000000001);
#5437=CIRCLE('',#14289,0.210000000000001);
#5438=CIRCLE('',#14292,0.210000000000001);
#5439=CIRCLE('',#14293,0.210000000000001);
#5440=CIRCLE('',#14296,0.210000000000001);
#5441=CIRCLE('',#14297,0.210000000000001);
#5442=CIRCLE('',#14300,0.210000000000001);
#5443=CIRCLE('',#14301,0.210000000000001);
#5444=CIRCLE('',#14304,0.165);
#5445=CIRCLE('',#14305,0.165);
#5446=CIRCLE('',#14308,0.165);
#5447=CIRCLE('',#14309,0.165);
#5448=CIRCLE('',#14312,0.165);
#5449=CIRCLE('',#14313,0.165);
#5450=CIRCLE('',#14316,1.11);
#5451=CIRCLE('',#14317,1.11);
#5452=CIRCLE('',#14327,0.21);
#5453=CIRCLE('',#14329,0.21);
#5454=CIRCLE('',#14330,0.21);
#5455=CIRCLE('',#14331,0.21);
#5456=CIRCLE('',#14333,0.21);
#5457=CIRCLE('',#14335,0.21);
#5458=CIRCLE('',#14336,0.21);
#5459=CIRCLE('',#14337,0.21);
#5460=CIRCLE('',#14339,0.21);
#5461=CIRCLE('',#14341,0.21);
#5462=CIRCLE('',#14342,0.21);
#5463=CIRCLE('',#14343,0.21);
#5464=CIRCLE('',#14345,0.21);
#5465=CIRCLE('',#14347,0.21);
#5466=CIRCLE('',#14348,0.21);
#5467=CIRCLE('',#14349,0.21);
#5468=CIRCLE('',#14391,0.285);
#5469=CIRCLE('',#14392,0.265);
#5470=CIRCLE('',#14394,0.265);
#5471=CIRCLE('',#14396,0.5);
#5472=CIRCLE('',#14398,0.5);
#5473=CIRCLE('',#14410,0.25);
#5474=CIRCLE('',#14411,0.24505);
#5475=CIRCLE('',#14413,0.25);
#5476=CIRCLE('',#14416,0.375);
#5477=CIRCLE('',#14418,0.425);
#5478=CIRCLE('',#14420,0.425);
#5479=CIRCLE('',#14422,0.395);
#5480=CIRCLE('',#14424,0.27);
#5481=CIRCLE('',#14426,0.24505);
#5482=CIRCLE('',#14430,0.457875);
#5483=CIRCLE('',#14439,0.457875);
#5484=CIRCLE('',#14441,0.625);
#5485=CIRCLE('',#14450,0.625);
#5486=CIRCLE('',#14453,1.9);
#5487=CIRCLE('',#14454,0.457875);
#5488=CIRCLE('',#14455,0.225);
#5489=CIRCLE('',#14456,0.225);
#5490=CIRCLE('',#14457,0.225);
#5491=CIRCLE('',#14459,0.225);
#5492=CIRCLE('',#14461,0.225);
#5493=CIRCLE('',#14463,0.225);
#5494=CIRCLE('',#14466,1.9);
#5495=CIRCLE('',#14467,1.1);
#5496=CIRCLE('',#14471,1.1);
#5497=CIRCLE('',#14475,0.3);
#5498=CIRCLE('',#14477,0.35);
#5499=CIRCLE('',#14479,0.35);
#5500=CIRCLE('',#14481,0.32);
#5501=CIRCLE('',#14483,0.22);
#5502=CIRCLE('',#14485,0.1954);
#5503=CIRCLE('',#14487,0.1954);
#5504=CIRCLE('',#14489,0.16);
#5505=CIRCLE('',#14501,0.375);
#5506=CIRCLE('',#14503,0.425);
#5507=CIRCLE('',#14505,0.425);
#5508=CIRCLE('',#14507,0.395);
#5509=CIRCLE('',#14509,0.27);
#5510=CIRCLE('',#14511,0.24505);
#5511=CIRCLE('',#14513,0.24505);
#5512=CIRCLE('',#14515,0.2);
#5513=CIRCLE('',#14548,0.5941);
#5514=CIRCLE('',#14612,0.415875);
#5515=CIRCLE('',#14614,0.415875);
#5516=CIRCLE('',#14677,0.6);
#5517=CIRCLE('',#14678,0.415875);
#5518=CIRCLE('',#14680,0.6);
#5519=CIRCLE('',#14685,1.);
#5520=CIRCLE('',#14689,1.);
#5521=CIRCLE('',#14691,1.);
#5522=CIRCLE('',#14692,1.);
#5523=CIRCLE('',#14695,1.35);
#5524=CIRCLE('',#14696,0.5941);
#5525=CIRCLE('',#14698,1.35);
#5526=CIRCLE('',#14703,1.01);
#5527=CIRCLE('',#14704,1.01);
#5528=CIRCLE('',#14706,1.35);
#5529=CIRCLE('',#14707,1.35);
#5530=CIRCLE('',#14712,0.210000000000001);
#5531=CIRCLE('',#14714,0.210000000000001);
#5532=CIRCLE('',#14717,1.005);
#5533=CIRCLE('',#14718,1.005);
#5534=CIRCLE('',#14720,1.5);
#5535=CIRCLE('',#14721,1.5);
#5536=CIRCLE('',#14726,0.25);
#5537=CIRCLE('',#14727,0.25);
#5538=CIRCLE('',#14729,0.210000000000001);
#5539=CIRCLE('',#14731,0.210000000000001);
#5540=CIRCLE('',#14737,3.5);
#5541=CIRCLE('',#14738,1.);
#5542=CIRCLE('',#14740,3.5);
#5543=CIRCLE('',#14741,1.5);
#5544=CIRCLE('',#14744,1.);
#5545=CIRCLE('',#14746,1.5);
#5546=CIRCLE('',#14750,0.33);
#5547=CIRCLE('',#14751,0.33);
#5548=CIRCLE('',#14753,0.4);
#5549=CIRCLE('',#14754,0.4);
#5550=CIRCLE('',#14759,0.405);
#5551=CIRCLE('',#14760,0.405);
#5552=CIRCLE('',#14762,0.9);
#5553=CIRCLE('',#14763,0.9);
#5554=CIRCLE('',#14786,0.22);
#5555=CIRCLE('',#14788,0.24505);
#5556=CIRCLE('',#14790,0.24505);
#5557=CIRCLE('',#14792,0.175);
#5558=CIRCLE('',#14796,0.32);
#5559=CIRCLE('',#14797,0.32);
#5560=CIRCLE('',#14799,0.6);
#5561=CIRCLE('',#14800,0.6);
#5562=CIRCLE('',#14805,0.45);
#5563=CIRCLE('',#14807,0.5);
#5564=CIRCLE('',#14809,0.5);
#5565=CIRCLE('',#14811,0.47);
#5566=CIRCLE('',#14813,0.32);
#5567=CIRCLE('',#14815,0.2942);
#5568=CIRCLE('',#14817,0.2942);
#5569=CIRCLE('',#14819,0.24);
#5570=VERTEX_POINT('',#18490);
#5571=VERTEX_POINT('',#18492);
#5572=VERTEX_POINT('',#18496);
#5573=VERTEX_POINT('',#18498);
#5574=VERTEX_POINT('',#18502);
#5575=VERTEX_POINT('',#18504);
#5576=VERTEX_POINT('',#18508);
#5577=VERTEX_POINT('',#18510);
#5578=VERTEX_POINT('',#18514);
#5579=VERTEX_POINT('',#18516);
#5580=VERTEX_POINT('',#18520);
#5581=VERTEX_POINT('',#18522);
#5582=VERTEX_POINT('',#18526);
#5583=VERTEX_POINT('',#18528);
#5584=VERTEX_POINT('',#18532);
#5585=VERTEX_POINT('',#18534);
#5586=VERTEX_POINT('',#18538);
#5587=VERTEX_POINT('',#18540);
#5588=VERTEX_POINT('',#18544);
#5589=VERTEX_POINT('',#18546);
#5590=VERTEX_POINT('',#18550);
#5591=VERTEX_POINT('',#18552);
#5592=VERTEX_POINT('',#18556);
#5593=VERTEX_POINT('',#18558);
#5594=VERTEX_POINT('',#18562);
#5595=VERTEX_POINT('',#18564);
#5596=VERTEX_POINT('',#18568);
#5597=VERTEX_POINT('',#18570);
#5598=VERTEX_POINT('',#18574);
#5599=VERTEX_POINT('',#18576);
#5600=VERTEX_POINT('',#18580);
#5601=VERTEX_POINT('',#18582);
#5602=VERTEX_POINT('',#18586);
#5603=VERTEX_POINT('',#18587);
#5604=VERTEX_POINT('',#18589);
#5605=VERTEX_POINT('',#18591);
#5606=VERTEX_POINT('',#18595);
#5607=VERTEX_POINT('',#18597);
#5608=VERTEX_POINT('',#18601);
#5609=VERTEX_POINT('',#18603);
#5610=VERTEX_POINT('',#18613);
#5611=VERTEX_POINT('',#18615);
#5612=VERTEX_POINT('',#18619);
#5613=VERTEX_POINT('',#18621);
#5614=VERTEX_POINT('',#18625);
#5615=VERTEX_POINT('',#18627);
#5616=VERTEX_POINT('',#18631);
#5617=VERTEX_POINT('',#18633);
#5618=VERTEX_POINT('',#18637);
#5619=VERTEX_POINT('',#18639);
#5620=VERTEX_POINT('',#18643);
#5621=VERTEX_POINT('',#18646);
#5622=VERTEX_POINT('',#18648);
#5623=VERTEX_POINT('',#18652);
#5624=VERTEX_POINT('',#18655);
#5625=VERTEX_POINT('',#18657);
#5626=VERTEX_POINT('',#18661);
#5627=VERTEX_POINT('',#18664);
#5628=VERTEX_POINT('',#18666);
#5629=VERTEX_POINT('',#18670);
#5630=VERTEX_POINT('',#18673);
#5631=VERTEX_POINT('',#18677);
#5632=VERTEX_POINT('',#18681);
#5633=VERTEX_POINT('',#18685);
#5634=VERTEX_POINT('',#18689);
#5635=VERTEX_POINT('',#18690);
#5636=VERTEX_POINT('',#18692);
#5637=VERTEX_POINT('',#18694);
#5638=VERTEX_POINT('',#18698);
#5639=VERTEX_POINT('',#18700);
#5640=VERTEX_POINT('',#18704);
#5641=VERTEX_POINT('',#18706);
#5642=VERTEX_POINT('',#18716);
#5643=VERTEX_POINT('',#18718);
#5644=VERTEX_POINT('',#18722);
#5645=VERTEX_POINT('',#18724);
#5646=VERTEX_POINT('',#18728);
#5647=VERTEX_POINT('',#18730);
#5648=VERTEX_POINT('',#18734);
#5649=VERTEX_POINT('',#18736);
#5650=VERTEX_POINT('',#18740);
#5651=VERTEX_POINT('',#18743);
#5652=VERTEX_POINT('',#18747);
#5653=VERTEX_POINT('',#18749);
#5654=VERTEX_POINT('',#18754);
#5655=VERTEX_POINT('',#18756);
#5656=VERTEX_POINT('',#18761);
#5657=VERTEX_POINT('',#18762);
#5658=VERTEX_POINT('',#18764);
#5659=VERTEX_POINT('',#18766);
#5660=VERTEX_POINT('',#18770);
#5661=VERTEX_POINT('',#18772);
#5662=VERTEX_POINT('',#18776);
#5663=VERTEX_POINT('',#18778);
#5664=VERTEX_POINT('',#18788);
#5665=VERTEX_POINT('',#18790);
#5666=VERTEX_POINT('',#18794);
#5667=VERTEX_POINT('',#18796);
#5668=VERTEX_POINT('',#18800);
#5669=VERTEX_POINT('',#18802);
#5670=VERTEX_POINT('',#18806);
#5671=VERTEX_POINT('',#18808);
#5672=VERTEX_POINT('',#18812);
#5673=VERTEX_POINT('',#18815);
#5674=VERTEX_POINT('',#18819);
#5675=VERTEX_POINT('',#18821);
#5676=VERTEX_POINT('',#18828);
#5677=VERTEX_POINT('',#18830);
#5678=VERTEX_POINT('',#18834);
#5679=VERTEX_POINT('',#18836);
#5680=VERTEX_POINT('',#18840);
#5681=VERTEX_POINT('',#18842);
#5682=VERTEX_POINT('',#18846);
#5683=VERTEX_POINT('',#18848);
#5684=VERTEX_POINT('',#18852);
#5685=VERTEX_POINT('',#18855);
#5686=VERTEX_POINT('',#18859);
#5687=VERTEX_POINT('',#18861);
#5688=VERTEX_POINT('',#18866);
#5689=VERTEX_POINT('',#18868);
#5690=VERTEX_POINT('',#18873);
#5691=VERTEX_POINT('',#18874);
#5692=VERTEX_POINT('',#18876);
#5693=VERTEX_POINT('',#18878);
#5694=VERTEX_POINT('',#18882);
#5695=VERTEX_POINT('',#18884);
#5696=VERTEX_POINT('',#18888);
#5697=VERTEX_POINT('',#18890);
#5698=VERTEX_POINT('',#18900);
#5699=VERTEX_POINT('',#18901);
#5700=VERTEX_POINT('',#18903);
#5701=VERTEX_POINT('',#18905);
#5702=VERTEX_POINT('',#18910);
#5703=VERTEX_POINT('',#18912);
#5704=VERTEX_POINT('',#18914);
#5705=VERTEX_POINT('',#18916);
#5706=VERTEX_POINT('',#18921);
#5707=VERTEX_POINT('',#18925);
#5708=VERTEX_POINT('',#18929);
#5709=VERTEX_POINT('',#18933);
#5710=VERTEX_POINT('',#18937);
#5711=VERTEX_POINT('',#18940);
#5712=VERTEX_POINT('',#18946);
#5713=VERTEX_POINT('',#18947);
#5714=VERTEX_POINT('',#18949);
#5715=VERTEX_POINT('',#18952);
#5716=VERTEX_POINT('',#18955);
#5717=VERTEX_POINT('',#18957);
#5718=VERTEX_POINT('',#18960);
#5719=VERTEX_POINT('',#18964);
#5720=VERTEX_POINT('',#18965);
#5721=VERTEX_POINT('',#18967);
#5722=VERTEX_POINT('',#18970);
#5723=VERTEX_POINT('',#18973);
#5724=VERTEX_POINT('',#18975);
#5725=VERTEX_POINT('',#18978);
#5726=VERTEX_POINT('',#18982);
#5727=VERTEX_POINT('',#18984);
#5728=VERTEX_POINT('',#18986);
#5729=VERTEX_POINT('',#18988);
#5730=VERTEX_POINT('',#18992);
#5731=VERTEX_POINT('',#18994);
#5732=VERTEX_POINT('',#18996);
#5733=VERTEX_POINT('',#18998);
#5734=VERTEX_POINT('',#19002);
#5735=VERTEX_POINT('',#19006);
#5736=VERTEX_POINT('',#19013);
#5737=VERTEX_POINT('',#19015);
#5738=VERTEX_POINT('',#19017);
#5739=VERTEX_POINT('',#19019);
#5740=VERTEX_POINT('',#19023);
#5741=VERTEX_POINT('',#19027);
#5742=VERTEX_POINT('',#19031);
#5743=VERTEX_POINT('',#19033);
#5744=VERTEX_POINT('',#19043);
#5745=VERTEX_POINT('',#19044);
#5746=VERTEX_POINT('',#19046);
#5747=VERTEX_POINT('',#19049);
#5748=VERTEX_POINT('',#19052);
#5749=VERTEX_POINT('',#19054);
#5750=VERTEX_POINT('',#19057);
#5751=VERTEX_POINT('',#19061);
#5752=VERTEX_POINT('',#19062);
#5753=VERTEX_POINT('',#19064);
#5754=VERTEX_POINT('',#19067);
#5755=VERTEX_POINT('',#19070);
#5756=VERTEX_POINT('',#19072);
#5757=VERTEX_POINT('',#19075);
#5758=VERTEX_POINT('',#19079);
#5759=VERTEX_POINT('',#19081);
#5760=VERTEX_POINT('',#19083);
#5761=VERTEX_POINT('',#19085);
#5762=VERTEX_POINT('',#19089);
#5763=VERTEX_POINT('',#19091);
#5764=VERTEX_POINT('',#19093);
#5765=VERTEX_POINT('',#19095);
#5766=VERTEX_POINT('',#19099);
#5767=VERTEX_POINT('',#19103);
#5768=VERTEX_POINT('',#19110);
#5769=VERTEX_POINT('',#19112);
#5770=VERTEX_POINT('',#19114);
#5771=VERTEX_POINT('',#19116);
#5772=VERTEX_POINT('',#19120);
#5773=VERTEX_POINT('',#19124);
#5774=VERTEX_POINT('',#19128);
#5775=VERTEX_POINT('',#19130);
#5776=VERTEX_POINT('',#19140);
#5777=VERTEX_POINT('',#19142);
#5778=VERTEX_POINT('',#19146);
#5779=VERTEX_POINT('',#19149);
#5780=VERTEX_POINT('',#19151);
#5781=VERTEX_POINT('',#19155);
#5782=VERTEX_POINT('',#19158);
#5783=VERTEX_POINT('',#19160);
#5784=VERTEX_POINT('',#19164);
#5785=VERTEX_POINT('',#19167);
#5786=VERTEX_POINT('',#19169);
#5787=VERTEX_POINT('',#19173);
#5788=VERTEX_POINT('',#19176);
#5789=VERTEX_POINT('',#19180);
#5790=VERTEX_POINT('',#19184);
#5791=VERTEX_POINT('',#19188);
#5792=VERTEX_POINT('',#19192);
#5793=VERTEX_POINT('',#19193);
#5794=VERTEX_POINT('',#19195);
#5795=VERTEX_POINT('',#19197);
#5796=VERTEX_POINT('',#19201);
#5797=VERTEX_POINT('',#19203);
#5798=VERTEX_POINT('',#19207);
#5799=VERTEX_POINT('',#19209);
#5800=VERTEX_POINT('',#19213);
#5801=VERTEX_POINT('',#19215);
#5802=VERTEX_POINT('',#19219);
#5803=VERTEX_POINT('',#19221);
#5804=VERTEX_POINT('',#19225);
#5805=VERTEX_POINT('',#19227);
#5806=VERTEX_POINT('',#19231);
#5807=VERTEX_POINT('',#19233);
#5808=VERTEX_POINT('',#19237);
#5809=VERTEX_POINT('',#19239);
#5810=VERTEX_POINT('',#19243);
#5811=VERTEX_POINT('',#19245);
#5812=VERTEX_POINT('',#19249);
#5813=VERTEX_POINT('',#19251);
#5814=VERTEX_POINT('',#19255);
#5815=VERTEX_POINT('',#19257);
#5816=VERTEX_POINT('',#19268);
#5817=VERTEX_POINT('',#19269);
#5818=VERTEX_POINT('',#19272);
#5819=VERTEX_POINT('',#19274);
#5820=VERTEX_POINT('',#19278);
#5821=VERTEX_POINT('',#19282);
#5822=VERTEX_POINT('',#19284);
#5823=VERTEX_POINT('',#19288);
#5824=VERTEX_POINT('',#19293);
#5825=VERTEX_POINT('',#19297);
#5826=VERTEX_POINT('',#19303);
#5827=VERTEX_POINT('',#19304);
#5828=VERTEX_POINT('',#19307);
#5829=VERTEX_POINT('',#19309);
#5830=VERTEX_POINT('',#19313);
#5831=VERTEX_POINT('',#19317);
#5832=VERTEX_POINT('',#19319);
#5833=VERTEX_POINT('',#19322);
#5834=VERTEX_POINT('',#19326);
#5835=VERTEX_POINT('',#19330);
#5836=VERTEX_POINT('',#19338);
#5837=VERTEX_POINT('',#19339);
#5838=VERTEX_POINT('',#19342);
#5839=VERTEX_POINT('',#19343);
#5840=VERTEX_POINT('',#19346);
#5841=VERTEX_POINT('',#19347);
#5842=VERTEX_POINT('',#19350);
#5843=VERTEX_POINT('',#19351);
#5844=VERTEX_POINT('',#19354);
#5845=VERTEX_POINT('',#19355);
#5846=VERTEX_POINT('',#19358);
#5847=VERTEX_POINT('',#19359);
#5848=VERTEX_POINT('',#19362);
#5849=VERTEX_POINT('',#19363);
#5850=VERTEX_POINT('',#19367);
#5851=VERTEX_POINT('',#19368);
#5852=VERTEX_POINT('',#19391);
#5853=VERTEX_POINT('',#19393);
#5854=VERTEX_POINT('',#19418);
#5855=VERTEX_POINT('',#19420);
#5856=VERTEX_POINT('',#19443);
#5857=VERTEX_POINT('',#19445);
#5858=VERTEX_POINT('',#19468);
#5859=VERTEX_POINT('',#19470);
#5860=VERTEX_POINT('',#19473);
#5861=VERTEX_POINT('',#19475);
#5862=VERTEX_POINT('',#19498);
#5863=VERTEX_POINT('',#19500);
#5864=VERTEX_POINT('',#19523);
#5865=VERTEX_POINT('',#19525);
#5866=VERTEX_POINT('',#19548);
#5867=VERTEX_POINT('',#19550);
#5868=VERTEX_POINT('',#19575);
#5869=VERTEX_POINT('',#19579);
#5870=VERTEX_POINT('',#19604);
#5871=VERTEX_POINT('',#19608);
#5872=VERTEX_POINT('',#19633);
#5873=VERTEX_POINT('',#19635);
#5874=VERTEX_POINT('',#19639);
#5875=VERTEX_POINT('',#19664);
#5876=VERTEX_POINT('',#19668);
#5877=VERTEX_POINT('',#19693);
#5878=VERTEX_POINT('',#19697);
#5879=VERTEX_POINT('',#19722);
#5880=VERTEX_POINT('',#19725);
#5881=VERTEX_POINT('',#19727);
#5882=VERTEX_POINT('',#19759);
#5883=VERTEX_POINT('',#19761);
#5884=VERTEX_POINT('',#19764);
#5885=VERTEX_POINT('',#19768);
#5886=VERTEX_POINT('',#19773);
#5887=VERTEX_POINT('',#19775);
#5888=VERTEX_POINT('',#19778);
#5889=VERTEX_POINT('',#19782);
#5890=VERTEX_POINT('',#19794);
#5891=VERTEX_POINT('',#19795);
#5892=VERTEX_POINT('',#19798);
#5893=VERTEX_POINT('',#19800);
#5894=VERTEX_POINT('',#19804);
#5895=VERTEX_POINT('',#19808);
#5896=VERTEX_POINT('',#19810);
#5897=VERTEX_POINT('',#19814);
#5898=VERTEX_POINT('',#19819);
#5899=VERTEX_POINT('',#19823);
#5900=VERTEX_POINT('',#19829);
#5901=VERTEX_POINT('',#19830);
#5902=VERTEX_POINT('',#19833);
#5903=VERTEX_POINT('',#19835);
#5904=VERTEX_POINT('',#19839);
#5905=VERTEX_POINT('',#19843);
#5906=VERTEX_POINT('',#19845);
#5907=VERTEX_POINT('',#19848);
#5908=VERTEX_POINT('',#19852);
#5909=VERTEX_POINT('',#19856);
#5910=VERTEX_POINT('',#19864);
#5911=VERTEX_POINT('',#19865);
#5912=VERTEX_POINT('',#19868);
#5913=VERTEX_POINT('',#19869);
#5914=VERTEX_POINT('',#19872);
#5915=VERTEX_POINT('',#19873);
#5916=VERTEX_POINT('',#19876);
#5917=VERTEX_POINT('',#19877);
#5918=VERTEX_POINT('',#19880);
#5919=VERTEX_POINT('',#19881);
#5920=VERTEX_POINT('',#19884);
#5921=VERTEX_POINT('',#19885);
#5922=VERTEX_POINT('',#19888);
#5923=VERTEX_POINT('',#19889);
#5924=VERTEX_POINT('',#19892);
#5925=VERTEX_POINT('',#19893);
#5926=VERTEX_POINT('',#19897);
#5927=VERTEX_POINT('',#19898);
#5928=VERTEX_POINT('',#19921);
#5929=VERTEX_POINT('',#19923);
#5930=VERTEX_POINT('',#19948);
#5931=VERTEX_POINT('',#19950);
#5932=VERTEX_POINT('',#19973);
#5933=VERTEX_POINT('',#19975);
#5934=VERTEX_POINT('',#19998);
#5935=VERTEX_POINT('',#20000);
#5936=VERTEX_POINT('',#20013);
#5937=VERTEX_POINT('',#20016);
#5938=VERTEX_POINT('',#20029);
#5939=VERTEX_POINT('',#20031);
#5940=VERTEX_POINT('',#20054);
#5941=VERTEX_POINT('',#20056);
#5942=VERTEX_POINT('',#20079);
#5943=VERTEX_POINT('',#20081);
#5944=VERTEX_POINT('',#20104);
#5945=VERTEX_POINT('',#20106);
#5946=VERTEX_POINT('',#20131);
#5947=VERTEX_POINT('',#20135);
#5948=VERTEX_POINT('',#20160);
#5949=VERTEX_POINT('',#20164);
#5950=VERTEX_POINT('',#20189);
#5951=VERTEX_POINT('',#20193);
#5952=VERTEX_POINT('',#20194);
#5953=VERTEX_POINT('',#20221);
#5954=VERTEX_POINT('',#20225);
#5955=VERTEX_POINT('',#20250);
#5956=VERTEX_POINT('',#20254);
#5957=VERTEX_POINT('',#20279);
#5958=VERTEX_POINT('',#20283);
#5959=VERTEX_POINT('',#20308);
#5960=VERTEX_POINT('',#20311);
#5961=VERTEX_POINT('',#20313);
#5962=VERTEX_POINT('',#20345);
#5963=VERTEX_POINT('',#20347);
#5964=VERTEX_POINT('',#20350);
#5965=VERTEX_POINT('',#20354);
#5966=VERTEX_POINT('',#20359);
#5967=VERTEX_POINT('',#20361);
#5968=VERTEX_POINT('',#20364);
#5969=VERTEX_POINT('',#20368);
#5970=VERTEX_POINT('',#20379);
#5971=VERTEX_POINT('',#20380);
#5972=VERTEX_POINT('',#20382);
#5973=VERTEX_POINT('',#20384);
#5974=VERTEX_POINT('',#20388);
#5975=VERTEX_POINT('',#20390);
#5976=VERTEX_POINT('',#20394);
#5977=VERTEX_POINT('',#20396);
#5978=VERTEX_POINT('',#20400);
#5979=VERTEX_POINT('',#20402);
#5980=VERTEX_POINT('',#20406);
#5981=VERTEX_POINT('',#20408);
#5982=VERTEX_POINT('',#20412);
#5983=VERTEX_POINT('',#20414);
#5984=VERTEX_POINT('',#20418);
#5985=VERTEX_POINT('',#20420);
#5986=VERTEX_POINT('',#20424);
#5987=VERTEX_POINT('',#20426);
#5988=VERTEX_POINT('',#20430);
#5989=VERTEX_POINT('',#20432);
#5990=VERTEX_POINT('',#20436);
#5991=VERTEX_POINT('',#20437);
#5992=VERTEX_POINT('',#20439);
#5993=VERTEX_POINT('',#20441);
#5994=VERTEX_POINT('',#20445);
#5995=VERTEX_POINT('',#20447);
#5996=VERTEX_POINT('',#20451);
#5997=VERTEX_POINT('',#20453);
#5998=VERTEX_POINT('',#20457);
#5999=VERTEX_POINT('',#20459);
#6000=VERTEX_POINT('',#20463);
#6001=VERTEX_POINT('',#20465);
#6002=VERTEX_POINT('',#20469);
#6003=VERTEX_POINT('',#20471);
#6004=VERTEX_POINT('',#20475);
#6005=VERTEX_POINT('',#20477);
#6006=VERTEX_POINT('',#20481);
#6007=VERTEX_POINT('',#20483);
#6008=VERTEX_POINT('',#20487);
#6009=VERTEX_POINT('',#20489);
#6010=VERTEX_POINT('',#20493);
#6011=VERTEX_POINT('',#20494);
#6012=VERTEX_POINT('',#20496);
#6013=VERTEX_POINT('',#20498);
#6014=VERTEX_POINT('',#20502);
#6015=VERTEX_POINT('',#20504);
#6016=VERTEX_POINT('',#20508);
#6017=VERTEX_POINT('',#20510);
#6018=VERTEX_POINT('',#20514);
#6019=VERTEX_POINT('',#20516);
#6020=VERTEX_POINT('',#20520);
#6021=VERTEX_POINT('',#20522);
#6022=VERTEX_POINT('',#20526);
#6023=VERTEX_POINT('',#20528);
#6024=VERTEX_POINT('',#20532);
#6025=VERTEX_POINT('',#20534);
#6026=VERTEX_POINT('',#20538);
#6027=VERTEX_POINT('',#20540);
#6028=VERTEX_POINT('',#20544);
#6029=VERTEX_POINT('',#20546);
#6030=VERTEX_POINT('',#20550);
#6031=VERTEX_POINT('',#20551);
#6032=VERTEX_POINT('',#20553);
#6033=VERTEX_POINT('',#20555);
#6034=VERTEX_POINT('',#20559);
#6035=VERTEX_POINT('',#20561);
#6036=VERTEX_POINT('',#20565);
#6037=VERTEX_POINT('',#20567);
#6038=VERTEX_POINT('',#20571);
#6039=VERTEX_POINT('',#20573);
#6040=VERTEX_POINT('',#20577);
#6041=VERTEX_POINT('',#20579);
#6042=VERTEX_POINT('',#20583);
#6043=VERTEX_POINT('',#20585);
#6044=VERTEX_POINT('',#20589);
#6045=VERTEX_POINT('',#20591);
#6046=VERTEX_POINT('',#20595);
#6047=VERTEX_POINT('',#20597);
#6048=VERTEX_POINT('',#20601);
#6049=VERTEX_POINT('',#20603);
#6050=VERTEX_POINT('',#20607);
#6051=VERTEX_POINT('',#20609);
#6052=VERTEX_POINT('',#20613);
#6053=VERTEX_POINT('',#20615);
#6054=VERTEX_POINT('',#20619);
#6055=VERTEX_POINT('',#20621);
#6056=VERTEX_POINT('',#20628);
#6057=VERTEX_POINT('',#20630);
#6058=VERTEX_POINT('',#20637);
#6059=VERTEX_POINT('',#20639);
#6060=VERTEX_POINT('',#20652);
#6061=VERTEX_POINT('',#20653);
#6062=VERTEX_POINT('',#20655);
#6063=VERTEX_POINT('',#20657);
#6064=VERTEX_POINT('',#20659);
#6065=VERTEX_POINT('',#20661);
#6066=VERTEX_POINT('',#20665);
#6067=VERTEX_POINT('',#20667);
#6068=VERTEX_POINT('',#20670);
#6069=VERTEX_POINT('',#20672);
#6070=VERTEX_POINT('',#20676);
#6071=VERTEX_POINT('',#20680);
#6072=VERTEX_POINT('',#20684);
#6073=VERTEX_POINT('',#20686);
#6074=VERTEX_POINT('',#20690);
#6075=VERTEX_POINT('',#20692);
#6076=VERTEX_POINT('',#20696);
#6077=VERTEX_POINT('',#20700);
#6078=VERTEX_POINT('',#20708);
#6079=VERTEX_POINT('',#20710);
#6080=VERTEX_POINT('',#20714);
#6081=VERTEX_POINT('',#20718);
#6082=VERTEX_POINT('',#20721);
#6083=VERTEX_POINT('',#20727);
#6084=VERTEX_POINT('',#20728);
#6085=VERTEX_POINT('',#20730);
#6086=VERTEX_POINT('',#20732);
#6087=VERTEX_POINT('',#20736);
#6088=VERTEX_POINT('',#20738);
#6089=VERTEX_POINT('',#20742);
#6090=VERTEX_POINT('',#20744);
#6091=VERTEX_POINT('',#20748);
#6092=VERTEX_POINT('',#20750);
#6093=VERTEX_POINT('',#20754);
#6094=VERTEX_POINT('',#20756);
#6095=VERTEX_POINT('',#20765);
#6096=VERTEX_POINT('',#20768);
#6097=VERTEX_POINT('',#20771);
#6098=VERTEX_POINT('',#20775);
#6099=VERTEX_POINT('',#20779);
#6100=VERTEX_POINT('',#20783);
#6101=VERTEX_POINT('',#20786);
#6102=VERTEX_POINT('',#20794);
#6103=VERTEX_POINT('',#20796);
#6104=VERTEX_POINT('',#20800);
#6105=VERTEX_POINT('',#20802);
#6106=VERTEX_POINT('',#20806);
#6107=VERTEX_POINT('',#20808);
#6108=VERTEX_POINT('',#20812);
#6109=VERTEX_POINT('',#20814);
#6110=VERTEX_POINT('',#20818);
#6111=VERTEX_POINT('',#20819);
#6112=VERTEX_POINT('',#20821);
#6113=VERTEX_POINT('',#20823);
#6114=VERTEX_POINT('',#20827);
#6115=VERTEX_POINT('',#20829);
#6116=VERTEX_POINT('',#20833);
#6117=VERTEX_POINT('',#20835);
#6118=VERTEX_POINT('',#20845);
#6119=VERTEX_POINT('',#20847);
#6120=VERTEX_POINT('',#20851);
#6121=VERTEX_POINT('',#20853);
#6122=VERTEX_POINT('',#20857);
#6123=VERTEX_POINT('',#20859);
#6124=VERTEX_POINT('',#20863);
#6125=VERTEX_POINT('',#20865);
#6126=VERTEX_POINT('',#20869);
#6127=VERTEX_POINT('',#20871);
#6128=VERTEX_POINT('',#20875);
#6129=VERTEX_POINT('',#20877);
#6130=VERTEX_POINT('',#20881);
#6131=VERTEX_POINT('',#20883);
#6132=VERTEX_POINT('',#20887);
#6133=VERTEX_POINT('',#20889);
#6134=VERTEX_POINT('',#20893);
#6135=VERTEX_POINT('',#20894);
#6136=VERTEX_POINT('',#20896);
#6137=VERTEX_POINT('',#20898);
#6138=VERTEX_POINT('',#20902);
#6139=VERTEX_POINT('',#20904);
#6140=VERTEX_POINT('',#20908);
#6141=VERTEX_POINT('',#20910);
#6142=VERTEX_POINT('',#20920);
#6143=VERTEX_POINT('',#20922);
#6144=VERTEX_POINT('',#20927);
#6145=VERTEX_POINT('',#20929);
#6146=VERTEX_POINT('',#20934);
#6147=VERTEX_POINT('',#20936);
#6148=VERTEX_POINT('',#20941);
#6149=VERTEX_POINT('',#20943);
#6150=VERTEX_POINT('',#20948);
#6151=VERTEX_POINT('',#20950);
#6152=VERTEX_POINT('',#20955);
#6153=VERTEX_POINT('',#20957);
#6154=VERTEX_POINT('',#20962);
#6155=VERTEX_POINT('',#20964);
#6156=VERTEX_POINT('',#20969);
#6157=VERTEX_POINT('',#20971);
#6158=VERTEX_POINT('',#20975);
#6159=VERTEX_POINT('',#20976);
#6160=VERTEX_POINT('',#20978);
#6161=VERTEX_POINT('',#20980);
#6162=VERTEX_POINT('',#20984);
#6163=VERTEX_POINT('',#20986);
#6164=VERTEX_POINT('',#20990);
#6165=VERTEX_POINT('',#20992);
#6166=VERTEX_POINT('',#21003);
#6167=VERTEX_POINT('',#21004);
#6168=VERTEX_POINT('',#21008);
#6169=VERTEX_POINT('',#21010);
#6170=VERTEX_POINT('',#21012);
#6171=VERTEX_POINT('',#21015);
#6172=VERTEX_POINT('',#21019);
#6173=VERTEX_POINT('',#21020);
#6174=VERTEX_POINT('',#21024);
#6175=VERTEX_POINT('',#21026);
#6176=VERTEX_POINT('',#21028);
#6177=VERTEX_POINT('',#21031);
#6178=VERTEX_POINT('',#21035);
#6179=VERTEX_POINT('',#21036);
#6180=VERTEX_POINT('',#21040);
#6181=VERTEX_POINT('',#21042);
#6182=VERTEX_POINT('',#21044);
#6183=VERTEX_POINT('',#21047);
#6184=VERTEX_POINT('',#21051);
#6185=VERTEX_POINT('',#21052);
#6186=VERTEX_POINT('',#21056);
#6187=VERTEX_POINT('',#21058);
#6188=VERTEX_POINT('',#21060);
#6189=VERTEX_POINT('',#21063);
#6190=VERTEX_POINT('',#21068);
#6191=VERTEX_POINT('',#21070);
#6192=VERTEX_POINT('',#21072);
#6193=VERTEX_POINT('',#21074);
#6194=VERTEX_POINT('',#21079);
#6195=VERTEX_POINT('',#21081);
#6196=VERTEX_POINT('',#21083);
#6197=VERTEX_POINT('',#21085);
#6198=VERTEX_POINT('',#21089);
#6199=VERTEX_POINT('',#21091);
#6200=VERTEX_POINT('',#21093);
#6201=VERTEX_POINT('',#21095);
#6202=VERTEX_POINT('',#21098);
#6203=VERTEX_POINT('',#21100);
#6204=VERTEX_POINT('',#21102);
#6205=VERTEX_POINT('',#21104);
#6206=VERTEX_POINT('',#21108);
#6207=VERTEX_POINT('',#21112);
#6208=VERTEX_POINT('',#21116);
#6209=VERTEX_POINT('',#21120);
#6210=VERTEX_POINT('',#21126);
#6211=VERTEX_POINT('',#21130);
#6212=VERTEX_POINT('',#21134);
#6213=VERTEX_POINT('',#21138);
#6214=VERTEX_POINT('',#21146);
#6215=VERTEX_POINT('',#21147);
#6216=VERTEX_POINT('',#21149);
#6217=VERTEX_POINT('',#21151);
#6218=VERTEX_POINT('',#21155);
#6219=VERTEX_POINT('',#21157);
#6220=VERTEX_POINT('',#21161);
#6221=VERTEX_POINT('',#21163);
#6222=VERTEX_POINT('',#21167);
#6223=VERTEX_POINT('',#21169);
#6224=VERTEX_POINT('',#21173);
#6225=VERTEX_POINT('',#21175);
#6226=VERTEX_POINT('',#21179);
#6227=VERTEX_POINT('',#21181);
#6228=VERTEX_POINT('',#21185);
#6229=VERTEX_POINT('',#21187);
#6230=VERTEX_POINT('',#21197);
#6231=VERTEX_POINT('',#21198);
#6232=VERTEX_POINT('',#21200);
#6233=VERTEX_POINT('',#21202);
#6234=VERTEX_POINT('',#21206);
#6235=VERTEX_POINT('',#21208);
#6236=VERTEX_POINT('',#21212);
#6237=VERTEX_POINT('',#21214);
#6238=VERTEX_POINT('',#21218);
#6239=VERTEX_POINT('',#21220);
#6240=VERTEX_POINT('',#21224);
#6241=VERTEX_POINT('',#21226);
#6242=VERTEX_POINT('',#21230);
#6243=VERTEX_POINT('',#21232);
#6244=VERTEX_POINT('',#21236);
#6245=VERTEX_POINT('',#21238);
#6246=VERTEX_POINT('',#21251);
#6247=VERTEX_POINT('',#21253);
#6248=VERTEX_POINT('',#21257);
#6249=VERTEX_POINT('',#21261);
#6250=VERTEX_POINT('',#21264);
#6251=VERTEX_POINT('',#21270);
#6252=VERTEX_POINT('',#21271);
#6253=VERTEX_POINT('',#21273);
#6254=VERTEX_POINT('',#21275);
#6255=VERTEX_POINT('',#21279);
#6256=VERTEX_POINT('',#21281);
#6257=VERTEX_POINT('',#21285);
#6258=VERTEX_POINT('',#21287);
#6259=VERTEX_POINT('',#21291);
#6260=VERTEX_POINT('',#21293);
#6261=VERTEX_POINT('',#21297);
#6262=VERTEX_POINT('',#21299);
#6263=VERTEX_POINT('',#21308);
#6264=VERTEX_POINT('',#21310);
#6265=VERTEX_POINT('',#21313);
#6266=VERTEX_POINT('',#21318);
#6267=VERTEX_POINT('',#21321);
#6268=VERTEX_POINT('',#21325);
#6269=VERTEX_POINT('',#21329);
#6270=VERTEX_POINT('',#21333);
#6271=VERTEX_POINT('',#21336);
#6272=VERTEX_POINT('',#21343);
#6273=VERTEX_POINT('',#21344);
#6274=VERTEX_POINT('',#21346);
#6275=VERTEX_POINT('',#21372);
#6276=VERTEX_POINT('',#21415);
#6277=VERTEX_POINT('',#21416);
#6278=VERTEX_POINT('',#21502);
#6279=VERTEX_POINT('',#21503);
#6280=VERTEX_POINT('',#21592);
#6281=VERTEX_POINT('',#21593);
#6282=VERTEX_POINT('',#21679);
#6283=VERTEX_POINT('',#21680);
#6284=VERTEX_POINT('',#21769);
#6285=VERTEX_POINT('',#21770);
#6286=VERTEX_POINT('',#21856);
#6287=VERTEX_POINT('',#21857);
#6288=VERTEX_POINT('',#21943);
#6289=VERTEX_POINT('',#21944);
#6290=VERTEX_POINT('',#22033);
#6291=VERTEX_POINT('',#22034);
#6292=VERTEX_POINT('',#22036);
#6293=VERTEX_POINT('',#22049);
#6294=VERTEX_POINT('',#22050);
#6295=VERTEX_POINT('',#22052);
#6296=VERTEX_POINT('',#22060);
#6297=VERTEX_POINT('',#22075);
#6298=VERTEX_POINT('',#22076);
#6299=VERTEX_POINT('',#22112);
#6300=VERTEX_POINT('',#22113);
#6301=VERTEX_POINT('',#22149);
#6302=VERTEX_POINT('',#22150);
#6303=VERTEX_POINT('',#22187);
#6304=VERTEX_POINT('',#22188);
#6305=VERTEX_POINT('',#22224);
#6306=VERTEX_POINT('',#22225);
#6307=VERTEX_POINT('',#22261);
#6308=VERTEX_POINT('',#22262);
#6309=VERTEX_POINT('',#22299);
#6310=VERTEX_POINT('',#22300);
#6311=VERTEX_POINT('',#22337);
#6312=VERTEX_POINT('',#22338);
#6313=VERTEX_POINT('',#22340);
#6314=VERTEX_POINT('',#22346);
#6315=VERTEX_POINT('',#23410);
#6316=VERTEX_POINT('',#23502);
#6317=VERTEX_POINT('',#23503);
#6318=VERTEX_POINT('',#23507);
#6319=VERTEX_POINT('',#23509);
#6320=VERTEX_POINT('',#23511);
#6321=VERTEX_POINT('',#23514);
#6322=VERTEX_POINT('',#23518);
#6323=VERTEX_POINT('',#23522);
#6324=VERTEX_POINT('',#23526);
#6325=VERTEX_POINT('',#23527);
#6326=VERTEX_POINT('',#23533);
#6327=VERTEX_POINT('',#23538);
#6328=VERTEX_POINT('',#23544);
#6329=VERTEX_POINT('',#23547);
#6330=VERTEX_POINT('',#23551);
#6331=VERTEX_POINT('',#23555);
#6332=VERTEX_POINT('',#23559);
#6333=VERTEX_POINT('',#23562);
#6334=VERTEX_POINT('',#23566);
#6335=VERTEX_POINT('',#23570);
#6336=VERTEX_POINT('',#23575);
#6337=VERTEX_POINT('',#23576);
#6338=VERTEX_POINT('',#23578);
#6339=VERTEX_POINT('',#23580);
#6340=VERTEX_POINT('',#23584);
#6341=VERTEX_POINT('',#23586);
#6342=VERTEX_POINT('',#23590);
#6343=VERTEX_POINT('',#23592);
#6344=VERTEX_POINT('',#23596);
#6345=VERTEX_POINT('',#23598);
#6346=VERTEX_POINT('',#23602);
#6347=VERTEX_POINT('',#23604);
#6348=VERTEX_POINT('',#23614);
#6349=VERTEX_POINT('',#23617);
#6350=VERTEX_POINT('',#23621);
#6351=VERTEX_POINT('',#23625);
#6352=VERTEX_POINT('',#23629);
#6353=VERTEX_POINT('',#23632);
#6354=VERTEX_POINT('',#23636);
#6355=VERTEX_POINT('',#23640);
#6356=VERTEX_POINT('',#23645);
#6357=VERTEX_POINT('',#23646);
#6358=VERTEX_POINT('',#23648);
#6359=VERTEX_POINT('',#23650);
#6360=VERTEX_POINT('',#23654);
#6361=VERTEX_POINT('',#23656);
#6362=VERTEX_POINT('',#23660);
#6363=VERTEX_POINT('',#23662);
#6364=VERTEX_POINT('',#23666);
#6365=VERTEX_POINT('',#23668);
#6366=VERTEX_POINT('',#23672);
#6367=VERTEX_POINT('',#23674);
#6368=VERTEX_POINT('',#23705);
#6369=VERTEX_POINT('',#23706);
#6370=VERTEX_POINT('',#23708);
#6371=VERTEX_POINT('',#23728);
#6372=VERTEX_POINT('',#23735);
#6373=VERTEX_POINT('',#23736);
#6374=VERTEX_POINT('',#23822);
#6375=VERTEX_POINT('',#23823);
#6376=VERTEX_POINT('',#23912);
#6377=VERTEX_POINT('',#23913);
#6378=VERTEX_POINT('',#23999);
#6379=VERTEX_POINT('',#24000);
#6380=VERTEX_POINT('',#24086);
#6381=VERTEX_POINT('',#24087);
#6382=VERTEX_POINT('',#24173);
#6383=VERTEX_POINT('',#24174);
#6384=VERTEX_POINT('',#24260);
#6385=VERTEX_POINT('',#24261);
#6386=VERTEX_POINT('',#24347);
#6387=VERTEX_POINT('',#24348);
#6388=VERTEX_POINT('',#24419);
#6389=VERTEX_POINT('',#24420);
#6390=VERTEX_POINT('',#24470);
#6391=VERTEX_POINT('',#24471);
#6392=VERTEX_POINT('',#24518);
#6393=VERTEX_POINT('',#24519);
#6394=VERTEX_POINT('',#24566);
#6395=VERTEX_POINT('',#24567);
#6396=VERTEX_POINT('',#24617);
#6397=VERTEX_POINT('',#24618);
#6398=VERTEX_POINT('',#24668);
#6399=VERTEX_POINT('',#24669);
#6400=VERTEX_POINT('',#24716);
#6401=VERTEX_POINT('',#24717);
#6402=VERTEX_POINT('',#24767);
#6403=VERTEX_POINT('',#24768);
#6404=VERTEX_POINT('',#24818);
#6405=VERTEX_POINT('',#24819);
#6406=VERTEX_POINT('',#24866);
#6407=VERTEX_POINT('',#24867);
#6408=VERTEX_POINT('',#24914);
#6409=VERTEX_POINT('',#24915);
#6410=VERTEX_POINT('',#24965);
#6411=VERTEX_POINT('',#24966);
#6412=VERTEX_POINT('',#25016);
#6413=VERTEX_POINT('',#25017);
#6414=VERTEX_POINT('',#25064);
#6415=VERTEX_POINT('',#25065);
#6416=VERTEX_POINT('',#25115);
#6417=VERTEX_POINT('',#25116);
#6418=VERTEX_POINT('',#25166);
#6419=VERTEX_POINT('',#25167);
#6420=VERTEX_POINT('',#25214);
#6421=VERTEX_POINT('',#25215);
#6422=VERTEX_POINT('',#25262);
#6423=VERTEX_POINT('',#25263);
#6424=VERTEX_POINT('',#25313);
#6425=VERTEX_POINT('',#25314);
#6426=VERTEX_POINT('',#25364);
#6427=VERTEX_POINT('',#25365);
#6428=VERTEX_POINT('',#25412);
#6429=VERTEX_POINT('',#25413);
#6430=VERTEX_POINT('',#25463);
#6431=VERTEX_POINT('',#25464);
#6432=VERTEX_POINT('',#25514);
#6433=VERTEX_POINT('',#25515);
#6434=VERTEX_POINT('',#25562);
#6435=VERTEX_POINT('',#25563);
#6436=VERTEX_POINT('',#25610);
#6437=VERTEX_POINT('',#25611);
#6438=VERTEX_POINT('',#25661);
#6439=VERTEX_POINT('',#25662);
#6440=VERTEX_POINT('',#25712);
#6441=VERTEX_POINT('',#25713);
#6442=VERTEX_POINT('',#25760);
#6443=VERTEX_POINT('',#25761);
#6444=VERTEX_POINT('',#25811);
#6445=VERTEX_POINT('',#25812);
#6446=VERTEX_POINT('',#25862);
#6447=VERTEX_POINT('',#25863);
#6448=VERTEX_POINT('',#25910);
#6449=VERTEX_POINT('',#25911);
#6450=VERTEX_POINT('',#25958);
#6451=VERTEX_POINT('',#25959);
#6452=VERTEX_POINT('',#26009);
#6453=VERTEX_POINT('',#26010);
#6454=VERTEX_POINT('',#26060);
#6455=VERTEX_POINT('',#26061);
#6456=VERTEX_POINT('',#26108);
#6457=VERTEX_POINT('',#26109);
#6458=VERTEX_POINT('',#26159);
#6459=VERTEX_POINT('',#26160);
#6460=VERTEX_POINT('',#26210);
#6461=VERTEX_POINT('',#26211);
#6462=VERTEX_POINT('',#26258);
#6463=VERTEX_POINT('',#26259);
#6464=VERTEX_POINT('',#26306);
#6465=VERTEX_POINT('',#26307);
#6466=VERTEX_POINT('',#26357);
#6467=VERTEX_POINT('',#26358);
#6468=VERTEX_POINT('',#26408);
#6469=VERTEX_POINT('',#26409);
#6470=VERTEX_POINT('',#26456);
#6471=VERTEX_POINT('',#26457);
#6472=VERTEX_POINT('',#26507);
#6473=VERTEX_POINT('',#26508);
#6474=VERTEX_POINT('',#26558);
#6475=VERTEX_POINT('',#26559);
#6476=VERTEX_POINT('',#26606);
#6477=VERTEX_POINT('',#26607);
#6478=VERTEX_POINT('',#26654);
#6479=VERTEX_POINT('',#26655);
#6480=VERTEX_POINT('',#26705);
#6481=VERTEX_POINT('',#26706);
#6482=VERTEX_POINT('',#26771);
#6483=VERTEX_POINT('',#26772);
#6484=VERTEX_POINT('',#26861);
#6485=VERTEX_POINT('',#26862);
#6486=VERTEX_POINT('',#26948);
#6487=VERTEX_POINT('',#26949);
#6488=VERTEX_POINT('',#27035);
#6489=VERTEX_POINT('',#27036);
#6490=VERTEX_POINT('',#27122);
#6491=VERTEX_POINT('',#27123);
#6492=VERTEX_POINT('',#27209);
#6493=VERTEX_POINT('',#27210);
#6494=VERTEX_POINT('',#27296);
#6495=VERTEX_POINT('',#27297);
#6496=VERTEX_POINT('',#27386);
#6497=VERTEX_POINT('',#27387);
#6498=VERTEX_POINT('',#27389);
#6499=VERTEX_POINT('',#27396);
#6500=VERTEX_POINT('',#27397);
#6501=VERTEX_POINT('',#27416);
#6502=VERTEX_POINT('',#27432);
#6503=VERTEX_POINT('',#27433);
#6504=VERTEX_POINT('',#27470);
#6505=VERTEX_POINT('',#27471);
#6506=VERTEX_POINT('',#27506);
#6507=VERTEX_POINT('',#27507);
#6508=VERTEX_POINT('',#27544);
#6509=VERTEX_POINT('',#27545);
#6510=VERTEX_POINT('',#27580);
#6511=VERTEX_POINT('',#27581);
#6512=VERTEX_POINT('',#27618);
#6513=VERTEX_POINT('',#27619);
#6514=VERTEX_POINT('',#27655);
#6515=VERTEX_POINT('',#27656);
#6516=VERTEX_POINT('',#27690);
#6517=VERTEX_POINT('',#27691);
#6518=VERTEX_POINT('',#27717);
#6519=VERTEX_POINT('',#27718);
#6520=VERTEX_POINT('',#27741);
#6521=VERTEX_POINT('',#27742);
#6522=VERTEX_POINT('',#27765);
#6523=VERTEX_POINT('',#27766);
#6524=VERTEX_POINT('',#27789);
#6525=VERTEX_POINT('',#27790);
#6526=VERTEX_POINT('',#27815);
#6527=VERTEX_POINT('',#27816);
#6528=VERTEX_POINT('',#27839);
#6529=VERTEX_POINT('',#27840);
#6530=VERTEX_POINT('',#27863);
#6531=VERTEX_POINT('',#27864);
#6532=VERTEX_POINT('',#27889);
#6533=VERTEX_POINT('',#27890);
#6534=VERTEX_POINT('',#27913);
#6535=VERTEX_POINT('',#27914);
#6536=VERTEX_POINT('',#27937);
#6537=VERTEX_POINT('',#27938);
#6538=VERTEX_POINT('',#27961);
#6539=VERTEX_POINT('',#27962);
#6540=VERTEX_POINT('',#27987);
#6541=VERTEX_POINT('',#27988);
#6542=VERTEX_POINT('',#28011);
#6543=VERTEX_POINT('',#28012);
#6544=VERTEX_POINT('',#28035);
#6545=VERTEX_POINT('',#28036);
#6546=VERTEX_POINT('',#28061);
#6547=VERTEX_POINT('',#28062);
#6548=VERTEX_POINT('',#28085);
#6549=VERTEX_POINT('',#28086);
#6550=VERTEX_POINT('',#28109);
#6551=VERTEX_POINT('',#28110);
#6552=VERTEX_POINT('',#28133);
#6553=VERTEX_POINT('',#28134);
#6554=VERTEX_POINT('',#28159);
#6555=VERTEX_POINT('',#28160);
#6556=VERTEX_POINT('',#28183);
#6557=VERTEX_POINT('',#28184);
#6558=VERTEX_POINT('',#28207);
#6559=VERTEX_POINT('',#28208);
#6560=VERTEX_POINT('',#28233);
#6561=VERTEX_POINT('',#28234);
#6562=VERTEX_POINT('',#28257);
#6563=VERTEX_POINT('',#28258);
#6564=VERTEX_POINT('',#28281);
#6565=VERTEX_POINT('',#28282);
#6566=VERTEX_POINT('',#28305);
#6567=VERTEX_POINT('',#28306);
#6568=VERTEX_POINT('',#28331);
#6569=VERTEX_POINT('',#28332);
#6570=VERTEX_POINT('',#28355);
#6571=VERTEX_POINT('',#28356);
#6572=VERTEX_POINT('',#28379);
#6573=VERTEX_POINT('',#28380);
#6574=VERTEX_POINT('',#28405);
#6575=VERTEX_POINT('',#28406);
#6576=VERTEX_POINT('',#28429);
#6577=VERTEX_POINT('',#28430);
#6578=VERTEX_POINT('',#28453);
#6579=VERTEX_POINT('',#28454);
#6580=VERTEX_POINT('',#28477);
#6581=VERTEX_POINT('',#28478);
#6582=VERTEX_POINT('',#28503);
#6583=VERTEX_POINT('',#28504);
#6584=VERTEX_POINT('',#28527);
#6585=VERTEX_POINT('',#28528);
#6586=VERTEX_POINT('',#28551);
#6587=VERTEX_POINT('',#28552);
#6588=VERTEX_POINT('',#28577);
#6589=VERTEX_POINT('',#28578);
#6590=VERTEX_POINT('',#28601);
#6591=VERTEX_POINT('',#28602);
#6592=VERTEX_POINT('',#28625);
#6593=VERTEX_POINT('',#28626);
#6594=VERTEX_POINT('',#28649);
#6595=VERTEX_POINT('',#28650);
#6596=VERTEX_POINT('',#28675);
#6597=VERTEX_POINT('',#28676);
#6598=VERTEX_POINT('',#28699);
#6599=VERTEX_POINT('',#28700);
#6600=VERTEX_POINT('',#28723);
#6601=VERTEX_POINT('',#28724);
#6602=VERTEX_POINT('',#28749);
#6603=VERTEX_POINT('',#28750);
#6604=VERTEX_POINT('',#28773);
#6605=VERTEX_POINT('',#28774);
#6606=VERTEX_POINT('',#28797);
#6607=VERTEX_POINT('',#28798);
#6608=VERTEX_POINT('',#28822);
#6609=VERTEX_POINT('',#28823);
#6610=VERTEX_POINT('',#28849);
#6611=VERTEX_POINT('',#28850);
#6612=VERTEX_POINT('',#28886);
#6613=VERTEX_POINT('',#28887);
#6614=VERTEX_POINT('',#28922);
#6615=VERTEX_POINT('',#28923);
#6616=VERTEX_POINT('',#28960);
#6617=VERTEX_POINT('',#28961);
#6618=VERTEX_POINT('',#28996);
#6619=VERTEX_POINT('',#28997);
#6620=VERTEX_POINT('',#29034);
#6621=VERTEX_POINT('',#29035);
#6622=VERTEX_POINT('',#29071);
#6623=VERTEX_POINT('',#29072);
#6624=VERTEX_POINT('',#29108);
#6625=VERTEX_POINT('',#29110);
#6626=VERTEX_POINT('',#29148);
#6627=VERTEX_POINT('',#29188);
#6628=VERTEX_POINT('',#31184);
#6629=VERTEX_POINT('',#33269);
#6630=VERTEX_POINT('',#33321);
#6631=VERTEX_POINT('',#33322);
#6632=VERTEX_POINT('',#33324);
#6633=VERTEX_POINT('',#33326);
#6634=VERTEX_POINT('',#33330);
#6635=VERTEX_POINT('',#33332);
#6636=VERTEX_POINT('',#33336);
#6637=VERTEX_POINT('',#33340);
#6638=VERTEX_POINT('',#33346);
#6639=VERTEX_POINT('',#33348);
#6640=VERTEX_POINT('',#33353);
#6641=VERTEX_POINT('',#33357);
#6642=VERTEX_POINT('',#33364);
#6643=VERTEX_POINT('',#33366);
#6644=VERTEX_POINT('',#33370);
#6645=VERTEX_POINT('',#33372);
#6646=VERTEX_POINT('',#33379);
#6647=VERTEX_POINT('',#33380);
#6648=VERTEX_POINT('',#33384);
#6649=VERTEX_POINT('',#33385);
#6650=VERTEX_POINT('',#33394);
#6651=VERTEX_POINT('',#33418);
#6652=VERTEX_POINT('',#33420);
#6653=VERTEX_POINT('',#33460);
#6654=VERTEX_POINT('',#33462);
#6655=VERTEX_POINT('',#33466);
#6656=VERTEX_POINT('',#33468);
#6657=VERTEX_POINT('',#33475);
#6658=VERTEX_POINT('',#33477);
#6659=VERTEX_POINT('',#33481);
#6660=VERTEX_POINT('',#33482);
#6661=VERTEX_POINT('',#33486);
#6662=VERTEX_POINT('',#33487);
#6663=VERTEX_POINT('',#33494);
#6664=VERTEX_POINT('',#33512);
#6665=VERTEX_POINT('',#33514);
#6666=VERTEX_POINT('',#33554);
#6667=VERTEX_POINT('',#33555);
#6668=VERTEX_POINT('',#33557);
#6669=VERTEX_POINT('',#33559);
#6670=VERTEX_POINT('',#33561);
#6671=VERTEX_POINT('',#33563);
#6672=VERTEX_POINT('',#33567);
#6673=VERTEX_POINT('',#33569);
#6674=VERTEX_POINT('',#33573);
#6675=VERTEX_POINT('',#33575);
#6676=VERTEX_POINT('',#33577);
#6677=VERTEX_POINT('',#33579);
#6678=VERTEX_POINT('',#33583);
#6679=VERTEX_POINT('',#33587);
#6680=VERTEX_POINT('',#33599);
#6681=VERTEX_POINT('',#33601);
#6682=VERTEX_POINT('',#33605);
#6683=VERTEX_POINT('',#33607);
#6684=VERTEX_POINT('',#33614);
#6685=VERTEX_POINT('',#33616);
#6686=VERTEX_POINT('',#33620);
#6687=VERTEX_POINT('',#33622);
#6688=VERTEX_POINT('',#33629);
#6689=VERTEX_POINT('',#33630);
#6690=VERTEX_POINT('',#33632);
#6691=VERTEX_POINT('',#33634);
#6692=VERTEX_POINT('',#33636);
#6693=VERTEX_POINT('',#33638);
#6694=VERTEX_POINT('',#33640);
#6695=VERTEX_POINT('',#33642);
#6696=VERTEX_POINT('',#33646);
#6697=VERTEX_POINT('',#33648);
#6698=VERTEX_POINT('',#33652);
#6699=VERTEX_POINT('',#33656);
#6700=VERTEX_POINT('',#33660);
#6701=VERTEX_POINT('',#33664);
#6702=VERTEX_POINT('',#33665);
#6703=VERTEX_POINT('',#33668);
#6704=VERTEX_POINT('',#33680);
#6705=VERTEX_POINT('',#33681);
#6706=VERTEX_POINT('',#33683);
#6707=VERTEX_POINT('',#33685);
#6708=VERTEX_POINT('',#33689);
#6709=VERTEX_POINT('',#33691);
#6710=VERTEX_POINT('',#33695);
#6711=VERTEX_POINT('',#33697);
#6712=VERTEX_POINT('',#33701);
#6713=VERTEX_POINT('',#33703);
#6714=VERTEX_POINT('',#33707);
#6715=VERTEX_POINT('',#33709);
#6716=VERTEX_POINT('',#33717);
#6717=VERTEX_POINT('',#33720);
#6718=VERTEX_POINT('',#33724);
#6719=VERTEX_POINT('',#33728);
#6720=VERTEX_POINT('',#33734);
#6721=VERTEX_POINT('',#33736);
#6722=VERTEX_POINT('',#33740);
#6723=VERTEX_POINT('',#33742);
#6724=VERTEX_POINT('',#33749);
#6725=VERTEX_POINT('',#33752);
#6726=VERTEX_POINT('',#33756);
#6727=VERTEX_POINT('',#33760);
#6728=VERTEX_POINT('',#33764);
#6729=VERTEX_POINT('',#33767);
#6730=VERTEX_POINT('',#33771);
#6731=VERTEX_POINT('',#33775);
#6732=VERTEX_POINT('',#33780);
#6733=VERTEX_POINT('',#33781);
#6734=VERTEX_POINT('',#33783);
#6735=VERTEX_POINT('',#33785);
#6736=VERTEX_POINT('',#33789);
#6737=VERTEX_POINT('',#33791);
#6738=VERTEX_POINT('',#33795);
#6739=VERTEX_POINT('',#33797);
#6740=VERTEX_POINT('',#33801);
#6741=VERTEX_POINT('',#33803);
#6742=VERTEX_POINT('',#33807);
#6743=VERTEX_POINT('',#33809);
#6744=EDGE_CURVE('',#5570,#5570,#5105,.T.);
#6745=EDGE_CURVE('',#5570,#5571,#3237,.T.);
#6746=EDGE_CURVE('',#5571,#5571,#5106,.T.);
#6747=EDGE_CURVE('',#5572,#5572,#5107,.T.);
#6748=EDGE_CURVE('',#5572,#5573,#3238,.T.);
#6749=EDGE_CURVE('',#5573,#5573,#5108,.T.);
#6750=EDGE_CURVE('',#5574,#5574,#5109,.T.);
#6751=EDGE_CURVE('',#5574,#5575,#3239,.T.);
#6752=EDGE_CURVE('',#5575,#5575,#5110,.T.);
#6753=EDGE_CURVE('',#5576,#5576,#5111,.T.);
#6754=EDGE_CURVE('',#5576,#5577,#3240,.T.);
#6755=EDGE_CURVE('',#5577,#5577,#5112,.T.);
#6756=EDGE_CURVE('',#5578,#5578,#5113,.T.);
#6757=EDGE_CURVE('',#5578,#5579,#3241,.T.);
#6758=EDGE_CURVE('',#5579,#5579,#5114,.T.);
#6759=EDGE_CURVE('',#5580,#5580,#5115,.T.);
#6760=EDGE_CURVE('',#5580,#5581,#3242,.T.);
#6761=EDGE_CURVE('',#5581,#5581,#5116,.T.);
#6762=EDGE_CURVE('',#5582,#5582,#5117,.T.);
#6763=EDGE_CURVE('',#5582,#5583,#3243,.T.);
#6764=EDGE_CURVE('',#5583,#5583,#5118,.T.);
#6765=EDGE_CURVE('',#5584,#5584,#5119,.T.);
#6766=EDGE_CURVE('',#5584,#5585,#3244,.T.);
#6767=EDGE_CURVE('',#5585,#5585,#5120,.T.);
#6768=EDGE_CURVE('',#5586,#5586,#5121,.T.);
#6769=EDGE_CURVE('',#5586,#5587,#3245,.T.);
#6770=EDGE_CURVE('',#5587,#5587,#5122,.T.);
#6771=EDGE_CURVE('',#5588,#5588,#5123,.T.);
#6772=EDGE_CURVE('',#5588,#5589,#3246,.T.);
#6773=EDGE_CURVE('',#5589,#5589,#5124,.T.);
#6774=EDGE_CURVE('',#5590,#5590,#5125,.T.);
#6775=EDGE_CURVE('',#5590,#5591,#3247,.T.);
#6776=EDGE_CURVE('',#5591,#5591,#5126,.T.);
#6777=EDGE_CURVE('',#5592,#5592,#5127,.T.);
#6778=EDGE_CURVE('',#5592,#5593,#3248,.T.);
#6779=EDGE_CURVE('',#5593,#5593,#5128,.T.);
#6780=EDGE_CURVE('',#5594,#5594,#5129,.T.);
#6781=EDGE_CURVE('',#5594,#5595,#3249,.T.);
#6782=EDGE_CURVE('',#5595,#5595,#5130,.T.);
#6783=EDGE_CURVE('',#5596,#5596,#5131,.T.);
#6784=EDGE_CURVE('',#5596,#5597,#3250,.T.);
#6785=EDGE_CURVE('',#5597,#5597,#5132,.T.);
#6786=EDGE_CURVE('',#5598,#5598,#5133,.T.);
#6787=EDGE_CURVE('',#5598,#5599,#3251,.T.);
#6788=EDGE_CURVE('',#5599,#5599,#5134,.T.);
#6789=EDGE_CURVE('',#5600,#5600,#5135,.T.);
#6790=EDGE_CURVE('',#5600,#5601,#3252,.T.);
#6791=EDGE_CURVE('',#5601,#5601,#5136,.T.);
#6792=EDGE_CURVE('',#5602,#5603,#3253,.T.);
#6793=EDGE_CURVE('',#5603,#5604,#3254,.T.);
#6794=EDGE_CURVE('',#5605,#5604,#3255,.T.);
#6795=EDGE_CURVE('',#5602,#5605,#3256,.T.);
#6796=EDGE_CURVE('',#5606,#5602,#3257,.T.);
#6797=EDGE_CURVE('',#5607,#5605,#3258,.T.);
#6798=EDGE_CURVE('',#5606,#5607,#3259,.T.);
#6799=EDGE_CURVE('',#5608,#5606,#3260,.T.);
#6800=EDGE_CURVE('',#5609,#5607,#3261,.T.);
#6801=EDGE_CURVE('',#5608,#5609,#3262,.T.);
#6802=EDGE_CURVE('',#5603,#5608,#3263,.T.);
#6803=EDGE_CURVE('',#5604,#5609,#3264,.T.);
#6804=EDGE_CURVE('',#5610,#5610,#5137,.T.);
#6805=EDGE_CURVE('',#5610,#5611,#3265,.T.);
#6806=EDGE_CURVE('',#5611,#5611,#5138,.T.);
#6807=EDGE_CURVE('',#5612,#5612,#5139,.T.);
#6808=EDGE_CURVE('',#5612,#5613,#3266,.T.);
#6809=EDGE_CURVE('',#5613,#5613,#5140,.T.);
#6810=EDGE_CURVE('',#5614,#5614,#5141,.T.);
#6811=EDGE_CURVE('',#5614,#5615,#3267,.T.);
#6812=EDGE_CURVE('',#5615,#5615,#5142,.T.);
#6813=EDGE_CURVE('',#5616,#5616,#5143,.T.);
#6814=EDGE_CURVE('',#5616,#5617,#3268,.T.);
#6815=EDGE_CURVE('',#5617,#5617,#5144,.T.);
#6816=EDGE_CURVE('',#5618,#5618,#5145,.T.);
#6817=EDGE_CURVE('',#5618,#5619,#3269,.T.);
#6818=EDGE_CURVE('',#5619,#5619,#5146,.T.);
#6819=EDGE_CURVE('',#5620,#5620,#5147,.T.);
#6820=EDGE_CURVE('',#5621,#5621,#5148,.T.);
#6821=EDGE_CURVE('',#5621,#5622,#3270,.T.);
#6822=EDGE_CURVE('',#5622,#5622,#5149,.T.);
#6823=EDGE_CURVE('',#5623,#5623,#5150,.T.);
#6824=EDGE_CURVE('',#5624,#5624,#5151,.T.);
#6825=EDGE_CURVE('',#5624,#5625,#3271,.T.);
#6826=EDGE_CURVE('',#5625,#5625,#5152,.T.);
#6827=EDGE_CURVE('',#5626,#5626,#5153,.T.);
#6828=EDGE_CURVE('',#5627,#5627,#5154,.T.);
#6829=EDGE_CURVE('',#5627,#5628,#3272,.T.);
#6830=EDGE_CURVE('',#5628,#5628,#5155,.T.);
#6831=EDGE_CURVE('',#5629,#5629,#5156,.T.);
#6832=EDGE_CURVE('',#5630,#5630,#5157,.T.);
#6833=EDGE_CURVE('',#5630,#5620,#3273,.T.);
#6834=EDGE_CURVE('',#5631,#5631,#5158,.T.);
#6835=EDGE_CURVE('',#5631,#5623,#3274,.T.);
#6836=EDGE_CURVE('',#5632,#5632,#5159,.T.);
#6837=EDGE_CURVE('',#5632,#5626,#3275,.T.);
#6838=EDGE_CURVE('',#5633,#5633,#5160,.T.);
#6839=EDGE_CURVE('',#5633,#5629,#3276,.T.);
#6840=EDGE_CURVE('',#5634,#5635,#3277,.T.);
#6841=EDGE_CURVE('',#5635,#5636,#3278,.T.);
#6842=EDGE_CURVE('',#5637,#5636,#3279,.T.);
#6843=EDGE_CURVE('',#5634,#5637,#3280,.T.);
#6844=EDGE_CURVE('',#5638,#5634,#3281,.T.);
#6845=EDGE_CURVE('',#5639,#5637,#3282,.T.);
#6846=EDGE_CURVE('',#5638,#5639,#3283,.T.);
#6847=EDGE_CURVE('',#5640,#5638,#3284,.T.);
#6848=EDGE_CURVE('',#5641,#5639,#3285,.T.);
#6849=EDGE_CURVE('',#5640,#5641,#3286,.T.);
#6850=EDGE_CURVE('',#5635,#5640,#3287,.T.);
#6851=EDGE_CURVE('',#5636,#5641,#3288,.T.);
#6852=EDGE_CURVE('',#5642,#5642,#5161,.T.);
#6853=EDGE_CURVE('',#5642,#5643,#3289,.T.);
#6854=EDGE_CURVE('',#5643,#5643,#5162,.T.);
#6855=EDGE_CURVE('',#5644,#5644,#5163,.T.);
#6856=EDGE_CURVE('',#5644,#5645,#3290,.T.);
#6857=EDGE_CURVE('',#5645,#5645,#5164,.T.);
#6858=EDGE_CURVE('',#5646,#5646,#5165,.T.);
#6859=EDGE_CURVE('',#5646,#5647,#3291,.T.);
#6860=EDGE_CURVE('',#5647,#5647,#5166,.T.);
#6861=EDGE_CURVE('',#5648,#5648,#5167,.T.);
#6862=EDGE_CURVE('',#5648,#5649,#3292,.T.);
#6863=EDGE_CURVE('',#5649,#5649,#5168,.T.);
#6864=EDGE_CURVE('',#5650,#5650,#5169,.T.);
#6865=EDGE_CURVE('',#5650,#5651,#3293,.T.);
#6866=EDGE_CURVE('',#5651,#5651,#5170,.T.);
#6867=EDGE_CURVE('',#5652,#5652,#5171,.T.);
#6868=EDGE_CURVE('',#5652,#5653,#3294,.T.);
#6869=EDGE_CURVE('',#5653,#5653,#5172,.T.);
#6870=EDGE_CURVE('',#5654,#5654,#5173,.T.);
#6871=EDGE_CURVE('',#5654,#5655,#3295,.T.);
#6872=EDGE_CURVE('',#5655,#5655,#5174,.T.);
#6873=EDGE_CURVE('',#5656,#5657,#3296,.T.);
#6874=EDGE_CURVE('',#5657,#5658,#3297,.T.);
#6875=EDGE_CURVE('',#5659,#5658,#3298,.T.);
#6876=EDGE_CURVE('',#5656,#5659,#3299,.T.);
#6877=EDGE_CURVE('',#5660,#5656,#3300,.T.);
#6878=EDGE_CURVE('',#5661,#5659,#3301,.T.);
#6879=EDGE_CURVE('',#5660,#5661,#3302,.T.);
#6880=EDGE_CURVE('',#5662,#5660,#3303,.T.);
#6881=EDGE_CURVE('',#5663,#5661,#3304,.T.);
#6882=EDGE_CURVE('',#5662,#5663,#3305,.T.);
#6883=EDGE_CURVE('',#5657,#5662,#3306,.T.);
#6884=EDGE_CURVE('',#5658,#5663,#3307,.T.);
#6885=EDGE_CURVE('',#5664,#5664,#5175,.T.);
#6886=EDGE_CURVE('',#5664,#5665,#3308,.T.);
#6887=EDGE_CURVE('',#5665,#5665,#5176,.T.);
#6888=EDGE_CURVE('',#5666,#5666,#5177,.T.);
#6889=EDGE_CURVE('',#5666,#5667,#3309,.T.);
#6890=EDGE_CURVE('',#5667,#5667,#5178,.T.);
#6891=EDGE_CURVE('',#5668,#5668,#5179,.T.);
#6892=EDGE_CURVE('',#5668,#5669,#3310,.T.);
#6893=EDGE_CURVE('',#5669,#5669,#5180,.T.);
#6894=EDGE_CURVE('',#5670,#5670,#5181,.T.);
#6895=EDGE_CURVE('',#5670,#5671,#3311,.T.);
#6896=EDGE_CURVE('',#5671,#5671,#5182,.T.);
#6897=EDGE_CURVE('',#5672,#5672,#5183,.T.);
#6898=EDGE_CURVE('',#5672,#5673,#3312,.T.);
#6899=EDGE_CURVE('',#5673,#5673,#5184,.T.);
#6900=EDGE_CURVE('',#5674,#5674,#5185,.T.);
#6901=EDGE_CURVE('',#5674,#5675,#3313,.T.);
#6902=EDGE_CURVE('',#5675,#5675,#5186,.T.);
#6903=EDGE_CURVE('',#5676,#5676,#5187,.T.);
#6904=EDGE_CURVE('',#5676,#5677,#3314,.T.);
#6905=EDGE_CURVE('',#5677,#5677,#5188,.T.);
#6906=EDGE_CURVE('',#5678,#5678,#5189,.T.);
#6907=EDGE_CURVE('',#5678,#5679,#3315,.T.);
#6908=EDGE_CURVE('',#5679,#5679,#5190,.T.);
#6909=EDGE_CURVE('',#5680,#5680,#5191,.T.);
#6910=EDGE_CURVE('',#5680,#5681,#3316,.T.);
#6911=EDGE_CURVE('',#5681,#5681,#5192,.T.);
#6912=EDGE_CURVE('',#5682,#5682,#5193,.T.);
#6913=EDGE_CURVE('',#5682,#5683,#3317,.T.);
#6914=EDGE_CURVE('',#5683,#5683,#5194,.T.);
#6915=EDGE_CURVE('',#5684,#5684,#5195,.T.);
#6916=EDGE_CURVE('',#5685,#5685,#5196,.T.);
#6917=EDGE_CURVE('',#5685,#5684,#3318,.T.);
#6918=EDGE_CURVE('',#5686,#5686,#5197,.T.);
#6919=EDGE_CURVE('',#5686,#5687,#3319,.T.);
#6920=EDGE_CURVE('',#5687,#5687,#5198,.T.);
#6921=EDGE_CURVE('',#5688,#5688,#5199,.T.);
#6922=EDGE_CURVE('',#5688,#5689,#3320,.T.);
#6923=EDGE_CURVE('',#5689,#5689,#5200,.T.);
#6924=EDGE_CURVE('',#5690,#5691,#3321,.T.);
#6925=EDGE_CURVE('',#5691,#5692,#3322,.T.);
#6926=EDGE_CURVE('',#5693,#5692,#3323,.T.);
#6927=EDGE_CURVE('',#5690,#5693,#3324,.T.);
#6928=EDGE_CURVE('',#5694,#5690,#3325,.T.);
#6929=EDGE_CURVE('',#5695,#5693,#3326,.T.);
#6930=EDGE_CURVE('',#5694,#5695,#3327,.T.);
#6931=EDGE_CURVE('',#5696,#5694,#3328,.T.);
#6932=EDGE_CURVE('',#5697,#5695,#3329,.T.);
#6933=EDGE_CURVE('',#5696,#5697,#3330,.T.);
#6934=EDGE_CURVE('',#5691,#5696,#3331,.T.);
#6935=EDGE_CURVE('',#5692,#5697,#3332,.T.);
#6936=EDGE_CURVE('',#5698,#5699,#3333,.T.);
#6937=EDGE_CURVE('',#5700,#5698,#3334,.T.);
#6938=EDGE_CURVE('',#5701,#5700,#3335,.T.);
#6939=EDGE_CURVE('',#5699,#5701,#3336,.T.);
#6940=EDGE_CURVE('',#5700,#5698,#5201,.T.);
#6941=EDGE_CURVE('',#5702,#5702,#5202,.T.);
#6942=EDGE_CURVE('',#5703,#5703,#5203,.T.);
#6943=EDGE_CURVE('',#5704,#5704,#5204,.T.);
#6944=EDGE_CURVE('',#5705,#5705,#5205,.T.);
#6945=EDGE_CURVE('',#5701,#5699,#5206,.T.);
#6946=EDGE_CURVE('',#5705,#5706,#3337,.T.);
#6947=EDGE_CURVE('',#5706,#5706,#5207,.T.);
#6948=EDGE_CURVE('',#5704,#5707,#3338,.T.);
#6949=EDGE_CURVE('',#5707,#5707,#5208,.T.);
#6950=EDGE_CURVE('',#5703,#5708,#3339,.T.);
#6951=EDGE_CURVE('',#5708,#5708,#5209,.T.);
#6952=EDGE_CURVE('',#5702,#5709,#3340,.T.);
#6953=EDGE_CURVE('',#5709,#5709,#5210,.T.);
#6954=EDGE_CURVE('',#5710,#5710,#5211,.T.);
#6955=EDGE_CURVE('',#5711,#5711,#5212,.T.);
#6956=EDGE_CURVE('',#5711,#5710,#3341,.T.);
#6957=EDGE_CURVE('',#5712,#5713,#3342,.T.);
#6958=EDGE_CURVE('',#5712,#5714,#5213,.T.);
#6959=EDGE_CURVE('',#5714,#5713,#5214,.T.);
#6960=EDGE_CURVE('',#5715,#5715,#5215,.T.);
#6961=EDGE_CURVE('',#5716,#5712,#3343,.T.);
#6962=EDGE_CURVE('',#5717,#5716,#5216,.T.);
#6963=EDGE_CURVE('',#5713,#5717,#3344,.T.);
#6964=EDGE_CURVE('',#5714,#5718,#3345,.T.);
#6965=EDGE_CURVE('',#5718,#5718,#5217,.T.);
#6966=EDGE_CURVE('',#5719,#5720,#3346,.T.);
#6967=EDGE_CURVE('',#5719,#5721,#5218,.T.);
#6968=EDGE_CURVE('',#5721,#5720,#5219,.T.);
#6969=EDGE_CURVE('',#5722,#5722,#5220,.T.);
#6970=EDGE_CURVE('',#5723,#5719,#3347,.T.);
#6971=EDGE_CURVE('',#5724,#5723,#5221,.T.);
#6972=EDGE_CURVE('',#5720,#5724,#3348,.T.);
#6973=EDGE_CURVE('',#5721,#5725,#3349,.T.);
#6974=EDGE_CURVE('',#5725,#5725,#5222,.T.);
#6975=EDGE_CURVE('',#5717,#5726,#3350,.T.);
#6976=EDGE_CURVE('',#5727,#5726,#3351,.T.);
#6977=EDGE_CURVE('',#5728,#5727,#3352,.T.);
#6978=EDGE_CURVE('',#5729,#5728,#3353,.T.);
#6979=EDGE_CURVE('',#5729,#5716,#3354,.T.);
#6980=EDGE_CURVE('',#5730,#5724,#3355,.T.);
#6981=EDGE_CURVE('',#5731,#5730,#3356,.T.);
#6982=EDGE_CURVE('',#5732,#5731,#3357,.T.);
#6983=EDGE_CURVE('',#5733,#5732,#3358,.T.);
#6984=EDGE_CURVE('',#5723,#5733,#3359,.T.);
#6985=EDGE_CURVE('',#5734,#5734,#5223,.T.);
#6986=EDGE_CURVE('',#5734,#5715,#3360,.T.);
#6987=EDGE_CURVE('',#5735,#5735,#5224,.T.);
#6988=EDGE_CURVE('',#5735,#5722,#3361,.T.);
#6989=EDGE_CURVE('',#5730,#5729,#3362,.T.);
#6990=EDGE_CURVE('',#5726,#5733,#3363,.T.);
#6991=EDGE_CURVE('',#5732,#5736,#3364,.T.);
#6992=EDGE_CURVE('',#5736,#5737,#3365,.T.);
#6993=EDGE_CURVE('',#5738,#5737,#3366,.T.);
#6994=EDGE_CURVE('',#5739,#5738,#3367,.T.);
#6995=EDGE_CURVE('',#5739,#5727,#3368,.T.);
#6996=EDGE_CURVE('',#5740,#5731,#3369,.T.);
#6997=EDGE_CURVE('',#5736,#5740,#3370,.T.);
#6998=EDGE_CURVE('',#5740,#5741,#3371,.T.);
#6999=EDGE_CURVE('',#5737,#5741,#3372,.T.);
#7000=EDGE_CURVE('',#5742,#5739,#3373,.T.);
#7001=EDGE_CURVE('',#5743,#5738,#3374,.T.);
#7002=EDGE_CURVE('',#5742,#5743,#3375,.T.);
#7003=EDGE_CURVE('',#5728,#5742,#3376,.T.);
#7004=EDGE_CURVE('',#5741,#5743,#3377,.T.);
#7005=EDGE_CURVE('',#5744,#5745,#3378,.T.);
#7006=EDGE_CURVE('',#5744,#5746,#5225,.T.);
#7007=EDGE_CURVE('',#5746,#5745,#5226,.T.);
#7008=EDGE_CURVE('',#5747,#5747,#5227,.T.);
#7009=EDGE_CURVE('',#5748,#5744,#3379,.T.);
#7010=EDGE_CURVE('',#5749,#5748,#5228,.T.);
#7011=EDGE_CURVE('',#5745,#5749,#3380,.T.);
#7012=EDGE_CURVE('',#5746,#5750,#3381,.T.);
#7013=EDGE_CURVE('',#5750,#5750,#5229,.T.);
#7014=EDGE_CURVE('',#5751,#5752,#3382,.T.);
#7015=EDGE_CURVE('',#5751,#5753,#5230,.T.);
#7016=EDGE_CURVE('',#5753,#5752,#5231,.T.);
#7017=EDGE_CURVE('',#5754,#5754,#5232,.T.);
#7018=EDGE_CURVE('',#5755,#5751,#3383,.T.);
#7019=EDGE_CURVE('',#5756,#5755,#5233,.T.);
#7020=EDGE_CURVE('',#5752,#5756,#3384,.T.);
#7021=EDGE_CURVE('',#5753,#5757,#3385,.T.);
#7022=EDGE_CURVE('',#5757,#5757,#5234,.T.);
#7023=EDGE_CURVE('',#5749,#5758,#3386,.T.);
#7024=EDGE_CURVE('',#5759,#5758,#3387,.T.);
#7025=EDGE_CURVE('',#5760,#5759,#3388,.T.);
#7026=EDGE_CURVE('',#5761,#5760,#3389,.T.);
#7027=EDGE_CURVE('',#5761,#5748,#3390,.T.);
#7028=EDGE_CURVE('',#5762,#5756,#3391,.T.);
#7029=EDGE_CURVE('',#5763,#5762,#3392,.T.);
#7030=EDGE_CURVE('',#5764,#5763,#3393,.T.);
#7031=EDGE_CURVE('',#5765,#5764,#3394,.T.);
#7032=EDGE_CURVE('',#5755,#5765,#3395,.T.);
#7033=EDGE_CURVE('',#5766,#5766,#5235,.T.);
#7034=EDGE_CURVE('',#5766,#5747,#3396,.T.);
#7035=EDGE_CURVE('',#5767,#5767,#5236,.T.);
#7036=EDGE_CURVE('',#5767,#5754,#3397,.T.);
#7037=EDGE_CURVE('',#5762,#5761,#3398,.T.);
#7038=EDGE_CURVE('',#5758,#5765,#3399,.T.);
#7039=EDGE_CURVE('',#5764,#5768,#3400,.T.);
#7040=EDGE_CURVE('',#5768,#5769,#3401,.T.);
#7041=EDGE_CURVE('',#5770,#5769,#3402,.T.);
#7042=EDGE_CURVE('',#5771,#5770,#3403,.T.);
#7043=EDGE_CURVE('',#5771,#5759,#3404,.T.);
#7044=EDGE_CURVE('',#5772,#5763,#3405,.T.);
#7045=EDGE_CURVE('',#5768,#5772,#3406,.T.);
#7046=EDGE_CURVE('',#5772,#5773,#3407,.T.);
#7047=EDGE_CURVE('',#5769,#5773,#3408,.T.);
#7048=EDGE_CURVE('',#5774,#5771,#3409,.T.);
#7049=EDGE_CURVE('',#5775,#5770,#3410,.T.);
#7050=EDGE_CURVE('',#5774,#5775,#3411,.T.);
#7051=EDGE_CURVE('',#5760,#5774,#3412,.T.);
#7052=EDGE_CURVE('',#5773,#5775,#3413,.T.);
#7053=EDGE_CURVE('',#5776,#5776,#5237,.T.);
#7054=EDGE_CURVE('',#5776,#5777,#3414,.T.);
#7055=EDGE_CURVE('',#5777,#5777,#5238,.T.);
#7056=EDGE_CURVE('',#5778,#5778,#5239,.T.);
#7057=EDGE_CURVE('',#5779,#5779,#5240,.T.);
#7058=EDGE_CURVE('',#5779,#5780,#3415,.T.);
#7059=EDGE_CURVE('',#5780,#5780,#5241,.T.);
#7060=EDGE_CURVE('',#5781,#5781,#5242,.T.);
#7061=EDGE_CURVE('',#5782,#5782,#5243,.T.);
#7062=EDGE_CURVE('',#5782,#5783,#3416,.T.);
#7063=EDGE_CURVE('',#5783,#5783,#5244,.T.);
#7064=EDGE_CURVE('',#5784,#5784,#5245,.T.);
#7065=EDGE_CURVE('',#5785,#5785,#5246,.T.);
#7066=EDGE_CURVE('',#5785,#5786,#3417,.T.);
#7067=EDGE_CURVE('',#5786,#5786,#5247,.T.);
#7068=EDGE_CURVE('',#5787,#5787,#5248,.T.);
#7069=EDGE_CURVE('',#5788,#5788,#5249,.T.);
#7070=EDGE_CURVE('',#5788,#5778,#3418,.T.);
#7071=EDGE_CURVE('',#5789,#5789,#5250,.T.);
#7072=EDGE_CURVE('',#5789,#5781,#3419,.T.);
#7073=EDGE_CURVE('',#5790,#5790,#5251,.T.);
#7074=EDGE_CURVE('',#5790,#5784,#3420,.T.);
#7075=EDGE_CURVE('',#5791,#5791,#5252,.T.);
#7076=EDGE_CURVE('',#5791,#5787,#3421,.T.);
#7077=EDGE_CURVE('',#5792,#5793,#3422,.T.);
#7078=EDGE_CURVE('',#5793,#5794,#3423,.T.);
#7079=EDGE_CURVE('',#5795,#5794,#3424,.T.);
#7080=EDGE_CURVE('',#5792,#5795,#3425,.T.);
#7081=EDGE_CURVE('',#5796,#5792,#3426,.T.);
#7082=EDGE_CURVE('',#5797,#5795,#3427,.T.);
#7083=EDGE_CURVE('',#5796,#5797,#3428,.T.);
#7084=EDGE_CURVE('',#5798,#5796,#3429,.T.);
#7085=EDGE_CURVE('',#5799,#5797,#3430,.T.);
#7086=EDGE_CURVE('',#5798,#5799,#3431,.T.);
#7087=EDGE_CURVE('',#5800,#5798,#3432,.T.);
#7088=EDGE_CURVE('',#5801,#5799,#3433,.T.);
#7089=EDGE_CURVE('',#5800,#5801,#3434,.T.);
#7090=EDGE_CURVE('',#5802,#5800,#3435,.T.);
#7091=EDGE_CURVE('',#5803,#5801,#3436,.T.);
#7092=EDGE_CURVE('',#5802,#5803,#3437,.T.);
#7093=EDGE_CURVE('',#5804,#5802,#3438,.T.);
#7094=EDGE_CURVE('',#5805,#5803,#3439,.T.);
#7095=EDGE_CURVE('',#5804,#5805,#3440,.T.);
#7096=EDGE_CURVE('',#5806,#5804,#3441,.T.);
#7097=EDGE_CURVE('',#5807,#5805,#3442,.T.);
#7098=EDGE_CURVE('',#5806,#5807,#3443,.T.);
#7099=EDGE_CURVE('',#5808,#5806,#3444,.T.);
#7100=EDGE_CURVE('',#5809,#5807,#3445,.T.);
#7101=EDGE_CURVE('',#5808,#5809,#3446,.T.);
#7102=EDGE_CURVE('',#5810,#5808,#3447,.T.);
#7103=EDGE_CURVE('',#5811,#5809,#3448,.T.);
#7104=EDGE_CURVE('',#5810,#5811,#3449,.T.);
#7105=EDGE_CURVE('',#5812,#5810,#3450,.T.);
#7106=EDGE_CURVE('',#5813,#5811,#3451,.T.);
#7107=EDGE_CURVE('',#5812,#5813,#3452,.T.);
#7108=EDGE_CURVE('',#5814,#5812,#3453,.T.);
#7109=EDGE_CURVE('',#5815,#5813,#3454,.T.);
#7110=EDGE_CURVE('',#5814,#5815,#3455,.T.);
#7111=EDGE_CURVE('',#5793,#5814,#3456,.T.);
#7112=EDGE_CURVE('',#5794,#5815,#3457,.T.);
#7113=EDGE_CURVE('',#5816,#5817,#5253,.T.);
#7114=EDGE_CURVE('',#5817,#5816,#5254,.T.);
#7115=EDGE_CURVE('',#5817,#5818,#5255,.T.);
#7116=EDGE_CURVE('',#5819,#5818,#5256,.T.);
#7117=EDGE_CURVE('',#5818,#5819,#5257,.T.);
#7118=EDGE_CURVE('',#5819,#5820,#3458,.T.);
#7119=EDGE_CURVE('',#5820,#5820,#5258,.T.);
#7120=EDGE_CURVE('',#5821,#5821,#5259,.T.);
#7121=EDGE_CURVE('',#5821,#5822,#3459,.T.);
#7122=EDGE_CURVE('',#5822,#5822,#5260,.T.);
#7123=EDGE_CURVE('',#5822,#5823,#3460,.T.);
#7124=EDGE_CURVE('',#5823,#5823,#5261,.T.);
#7125=EDGE_CURVE('',#5824,#5824,#5262,.T.);
#7126=EDGE_CURVE('',#5824,#5816,#3461,.T.);
#7127=EDGE_CURVE('',#5825,#5825,#5263,.T.);
#7128=EDGE_CURVE('',#5825,#5821,#3462,.T.);
#7129=EDGE_CURVE('',#5826,#5827,#5264,.T.);
#7130=EDGE_CURVE('',#5827,#5826,#5265,.T.);
#7131=EDGE_CURVE('',#5827,#5828,#5266,.T.);
#7132=EDGE_CURVE('',#5829,#5828,#5267,.T.);
#7133=EDGE_CURVE('',#5828,#5829,#5268,.T.);
#7134=EDGE_CURVE('',#5830,#5830,#5269,.T.);
#7135=EDGE_CURVE('',#5830,#5829,#3463,.T.);
#7136=EDGE_CURVE('',#5831,#5831,#5270,.T.);
#7137=EDGE_CURVE('',#5832,#5832,#5271,.T.);
#7138=EDGE_CURVE('',#5833,#5833,#5272,.T.);
#7139=EDGE_CURVE('',#5833,#5831,#3464,.T.);
#7140=EDGE_CURVE('',#5834,#5834,#5273,.T.);
#7141=EDGE_CURVE('',#5834,#5833,#3465,.T.);
#7142=EDGE_CURVE('',#5835,#5835,#5274,.T.);
#7143=EDGE_CURVE('',#5835,#5834,#3466,.T.);
#7144=EDGE_CURVE('',#5826,#5832,#3467,.T.);
#7145=EDGE_CURVE('',#5836,#5837,#5275,.T.);
#7146=EDGE_CURVE('',#5838,#5839,#5276,.T.);
#7147=EDGE_CURVE('',#5840,#5841,#5277,.T.);
#7148=EDGE_CURVE('',#5842,#5843,#5278,.T.);
#7149=EDGE_CURVE('',#5844,#5845,#5279,.T.);
#7150=EDGE_CURVE('',#5846,#5847,#5280,.T.);
#7151=EDGE_CURVE('',#5848,#5849,#5281,.T.);
#7152=EDGE_CURVE('',#5850,#5851,#403,.T.);
#7153=EDGE_CURVE('',#5852,#5850,#5282,.T.);
#7154=EDGE_CURVE('',#5853,#5852,#404,.T.);
#7155=EDGE_CURVE('',#5851,#5853,#5283,.T.);
#7156=EDGE_CURVE('',#5854,#5852,#5284,.T.);
#7157=EDGE_CURVE('',#5854,#5855,#405,.T.);
#7158=EDGE_CURVE('',#5856,#5855,#5285,.T.);
#7159=EDGE_CURVE('',#5856,#5857,#406,.T.);
#7160=EDGE_CURVE('',#5858,#5857,#5286,.T.);
#7161=EDGE_CURVE('',#5858,#5859,#3468,.T.);
#7162=EDGE_CURVE('',#5859,#5859,#5287,.T.);
#7163=EDGE_CURVE('',#5860,#5858,#5288,.T.);
#7164=EDGE_CURVE('',#5860,#5861,#407,.T.);
#7165=EDGE_CURVE('',#5862,#5861,#5289,.T.);
#7166=EDGE_CURVE('',#5862,#5863,#408,.T.);
#7167=EDGE_CURVE('',#5864,#5863,#5290,.T.);
#7168=EDGE_CURVE('',#5864,#5865,#409,.T.);
#7169=EDGE_CURVE('',#5866,#5865,#5291,.T.);
#7170=EDGE_CURVE('',#5866,#5867,#410,.T.);
#7171=EDGE_CURVE('',#5853,#5867,#5292,.T.);
#7172=EDGE_CURVE('',#5850,#5868,#5293,.T.);
#7173=EDGE_CURVE('',#5868,#5854,#5294,.T.);
#7174=EDGE_CURVE('',#5869,#5868,#411,.T.);
#7175=EDGE_CURVE('',#5855,#5869,#5295,.T.);
#7176=EDGE_CURVE('',#5869,#5870,#5296,.T.);
#7177=EDGE_CURVE('',#5870,#5856,#5297,.T.);
#7178=EDGE_CURVE('',#5871,#5870,#412,.T.);
#7179=EDGE_CURVE('',#5857,#5871,#5298,.T.);
#7180=EDGE_CURVE('',#5871,#5872,#5299,.T.);
#7181=EDGE_CURVE('',#5872,#5873,#5300,.T.);
#7182=EDGE_CURVE('',#5873,#5860,#5301,.T.);
#7183=EDGE_CURVE('',#5874,#5873,#413,.T.);
#7184=EDGE_CURVE('',#5861,#5874,#5302,.T.);
#7185=EDGE_CURVE('',#5874,#5875,#5303,.T.);
#7186=EDGE_CURVE('',#5875,#5862,#5304,.T.);
#7187=EDGE_CURVE('',#5876,#5875,#414,.T.);
#7188=EDGE_CURVE('',#5863,#5876,#5305,.T.);
#7189=EDGE_CURVE('',#5876,#5877,#5306,.T.);
#7190=EDGE_CURVE('',#5877,#5864,#5307,.T.);
#7191=EDGE_CURVE('',#5878,#5877,#415,.T.);
#7192=EDGE_CURVE('',#5865,#5878,#5308,.T.);
#7193=EDGE_CURVE('',#5879,#5879,#5309,.T.);
#7194=EDGE_CURVE('',#5879,#5872,#3469,.T.);
#7195=EDGE_CURVE('',#5880,#5851,#5310,.T.);
#7196=EDGE_CURVE('',#5880,#5881,#416,.T.);
#7197=EDGE_CURVE('',#5878,#5881,#5311,.T.);
#7198=EDGE_CURVE('',#5867,#5880,#5312,.T.);
#7199=EDGE_CURVE('',#5881,#5866,#5313,.T.);
#7200=EDGE_CURVE('',#5882,#5882,#5314,.T.);
#7201=EDGE_CURVE('',#5883,#5883,#5315,.T.);
#7202=EDGE_CURVE('',#5884,#5884,#5316,.T.);
#7203=EDGE_CURVE('',#5884,#5882,#3470,.T.);
#7204=EDGE_CURVE('',#5885,#5885,#5317,.T.);
#7205=EDGE_CURVE('',#5885,#5883,#3471,.T.);
#7206=EDGE_CURVE('',#5886,#5886,#5318,.T.);
#7207=EDGE_CURVE('',#5887,#5887,#5319,.T.);
#7208=EDGE_CURVE('',#5888,#5888,#5320,.T.);
#7209=EDGE_CURVE('',#5888,#5886,#3472,.T.);
#7210=EDGE_CURVE('',#5889,#5889,#5321,.T.);
#7211=EDGE_CURVE('',#5889,#5887,#3473,.T.);
#7212=EDGE_CURVE('',#5890,#5891,#5322,.T.);
#7213=EDGE_CURVE('',#5891,#5890,#5323,.T.);
#7214=EDGE_CURVE('',#5891,#5892,#5324,.T.);
#7215=EDGE_CURVE('',#5893,#5892,#5325,.T.);
#7216=EDGE_CURVE('',#5892,#5893,#5326,.T.);
#7217=EDGE_CURVE('',#5893,#5894,#3474,.T.);
#7218=EDGE_CURVE('',#5894,#5894,#5327,.T.);
#7219=EDGE_CURVE('',#5895,#5895,#5328,.T.);
#7220=EDGE_CURVE('',#5895,#5896,#3475,.T.);
#7221=EDGE_CURVE('',#5896,#5896,#5329,.T.);
#7222=EDGE_CURVE('',#5896,#5897,#3476,.T.);
#7223=EDGE_CURVE('',#5897,#5897,#5330,.T.);
#7224=EDGE_CURVE('',#5898,#5898,#5331,.T.);
#7225=EDGE_CURVE('',#5898,#5890,#3477,.T.);
#7226=EDGE_CURVE('',#5899,#5899,#5332,.T.);
#7227=EDGE_CURVE('',#5899,#5895,#3478,.T.);
#7228=EDGE_CURVE('',#5900,#5901,#5333,.T.);
#7229=EDGE_CURVE('',#5901,#5900,#5334,.T.);
#7230=EDGE_CURVE('',#5901,#5902,#5335,.T.);
#7231=EDGE_CURVE('',#5903,#5902,#5336,.T.);
#7232=EDGE_CURVE('',#5902,#5903,#5337,.T.);
#7233=EDGE_CURVE('',#5904,#5904,#5338,.T.);
#7234=EDGE_CURVE('',#5904,#5903,#3479,.T.);
#7235=EDGE_CURVE('',#5905,#5905,#5339,.T.);
#7236=EDGE_CURVE('',#5906,#5906,#5340,.T.);
#7237=EDGE_CURVE('',#5907,#5907,#5341,.T.);
#7238=EDGE_CURVE('',#5907,#5905,#3480,.T.);
#7239=EDGE_CURVE('',#5908,#5908,#5342,.T.);
#7240=EDGE_CURVE('',#5908,#5907,#3481,.T.);
#7241=EDGE_CURVE('',#5909,#5909,#5343,.T.);
#7242=EDGE_CURVE('',#5909,#5908,#3482,.T.);
#7243=EDGE_CURVE('',#5900,#5906,#3483,.T.);
#7244=EDGE_CURVE('',#5910,#5911,#5344,.T.);
#7245=EDGE_CURVE('',#5912,#5913,#5345,.T.);
#7246=EDGE_CURVE('',#5914,#5915,#5346,.T.);
#7247=EDGE_CURVE('',#5916,#5917,#5347,.T.);
#7248=EDGE_CURVE('',#5918,#5919,#5348,.T.);
#7249=EDGE_CURVE('',#5920,#5921,#5349,.T.);
#7250=EDGE_CURVE('',#5922,#5923,#5350,.T.);
#7251=EDGE_CURVE('',#5924,#5925,#5351,.T.);
#7252=EDGE_CURVE('',#5926,#5927,#417,.T.);
#7253=EDGE_CURVE('',#5928,#5926,#5352,.T.);
#7254=EDGE_CURVE('',#5929,#5928,#418,.T.);
#7255=EDGE_CURVE('',#5927,#5929,#5353,.T.);
#7256=EDGE_CURVE('',#5930,#5928,#5354,.T.);
#7257=EDGE_CURVE('',#5930,#5931,#419,.T.);
#7258=EDGE_CURVE('',#5932,#5931,#5355,.T.);
#7259=EDGE_CURVE('',#5932,#5933,#420,.T.);
#7260=EDGE_CURVE('',#5934,#5933,#5356,.T.);
#7261=EDGE_CURVE('',#5934,#5935,#421,.T.);
#7262=EDGE_CURVE('',#5935,#5936,#3484,.T.);
#7263=EDGE_CURVE('',#5936,#5936,#5357,.T.);
#7264=EDGE_CURVE('',#5935,#5937,#422,.T.);
#7265=EDGE_CURVE('',#5938,#5937,#5358,.T.);
#7266=EDGE_CURVE('',#5938,#5939,#423,.T.);
#7267=EDGE_CURVE('',#5940,#5939,#5359,.T.);
#7268=EDGE_CURVE('',#5940,#5941,#424,.T.);
#7269=EDGE_CURVE('',#5942,#5941,#5360,.T.);
#7270=EDGE_CURVE('',#5942,#5943,#425,.T.);
#7271=EDGE_CURVE('',#5944,#5943,#5361,.T.);
#7272=EDGE_CURVE('',#5944,#5945,#426,.T.);
#7273=EDGE_CURVE('',#5929,#5945,#5362,.T.);
#7274=EDGE_CURVE('',#5926,#5946,#5363,.T.);
#7275=EDGE_CURVE('',#5946,#5930,#5364,.T.);
#7276=EDGE_CURVE('',#5947,#5946,#427,.T.);
#7277=EDGE_CURVE('',#5931,#5947,#5365,.T.);
#7278=EDGE_CURVE('',#5947,#5948,#5366,.T.);
#7279=EDGE_CURVE('',#5948,#5932,#5367,.T.);
#7280=EDGE_CURVE('',#5949,#5948,#428,.T.);
#7281=EDGE_CURVE('',#5933,#5949,#5368,.T.);
#7282=EDGE_CURVE('',#5949,#5950,#5369,.T.);
#7283=EDGE_CURVE('',#5950,#5934,#5370,.T.);
#7284=EDGE_CURVE('',#5951,#5952,#429,.T.);
#7285=EDGE_CURVE('',#5937,#5951,#5371,.T.);
#7286=EDGE_CURVE('',#5952,#5950,#430,.T.);
#7287=EDGE_CURVE('',#5951,#5953,#5372,.T.);
#7288=EDGE_CURVE('',#5953,#5938,#5373,.T.);
#7289=EDGE_CURVE('',#5954,#5953,#431,.T.);
#7290=EDGE_CURVE('',#5939,#5954,#5374,.T.);
#7291=EDGE_CURVE('',#5954,#5955,#5375,.T.);
#7292=EDGE_CURVE('',#5955,#5940,#5376,.T.);
#7293=EDGE_CURVE('',#5956,#5955,#432,.T.);
#7294=EDGE_CURVE('',#5941,#5956,#5377,.T.);
#7295=EDGE_CURVE('',#5956,#5957,#5378,.T.);
#7296=EDGE_CURVE('',#5957,#5942,#5379,.T.);
#7297=EDGE_CURVE('',#5958,#5957,#433,.T.);
#7298=EDGE_CURVE('',#5943,#5958,#5380,.T.);
#7299=EDGE_CURVE('',#5959,#5959,#5381,.T.);
#7300=EDGE_CURVE('',#5959,#5952,#3485,.T.);
#7301=EDGE_CURVE('',#5960,#5927,#5382,.T.);
#7302=EDGE_CURVE('',#5960,#5961,#434,.T.);
#7303=EDGE_CURVE('',#5958,#5961,#5383,.T.);
#7304=EDGE_CURVE('',#5945,#5960,#5384,.T.);
#7305=EDGE_CURVE('',#5961,#5944,#5385,.T.);
#7306=EDGE_CURVE('',#5962,#5962,#5386,.T.);
#7307=EDGE_CURVE('',#5963,#5963,#5387,.T.);
#7308=EDGE_CURVE('',#5964,#5964,#5388,.T.);
#7309=EDGE_CURVE('',#5964,#5962,#3486,.T.);
#7310=EDGE_CURVE('',#5965,#5965,#5389,.T.);
#7311=EDGE_CURVE('',#5965,#5963,#3487,.T.);
#7312=EDGE_CURVE('',#5966,#5966,#5390,.T.);
#7313=EDGE_CURVE('',#5967,#5967,#5391,.T.);
#7314=EDGE_CURVE('',#5968,#5968,#5392,.T.);
#7315=EDGE_CURVE('',#5968,#5966,#3488,.T.);
#7316=EDGE_CURVE('',#5969,#5969,#5393,.T.);
#7317=EDGE_CURVE('',#5969,#5967,#3489,.T.);
#7318=EDGE_CURVE('',#5970,#5971,#3490,.T.);
#7319=EDGE_CURVE('',#5970,#5972,#3491,.T.);
#7320=EDGE_CURVE('',#5973,#5972,#3492,.T.);
#7321=EDGE_CURVE('',#5971,#5973,#3493,.T.);
#7322=EDGE_CURVE('',#5974,#5970,#3494,.T.);
#7323=EDGE_CURVE('',#5974,#5975,#3495,.T.);
#7324=EDGE_CURVE('',#5972,#5975,#3496,.T.);
#7325=EDGE_CURVE('',#5976,#5974,#3497,.T.);
#7326=EDGE_CURVE('',#5976,#5977,#3498,.T.);
#7327=EDGE_CURVE('',#5975,#5977,#3499,.T.);
#7328=EDGE_CURVE('',#5978,#5976,#3500,.T.);
#7329=EDGE_CURVE('',#5978,#5979,#3501,.T.);
#7330=EDGE_CURVE('',#5977,#5979,#3502,.T.);
#7331=EDGE_CURVE('',#5980,#5978,#3503,.T.);
#7332=EDGE_CURVE('',#5980,#5981,#3504,.T.);
#7333=EDGE_CURVE('',#5979,#5981,#3505,.T.);
#7334=EDGE_CURVE('',#5982,#5980,#3506,.T.);
#7335=EDGE_CURVE('',#5982,#5983,#3507,.T.);
#7336=EDGE_CURVE('',#5981,#5983,#3508,.T.);
#7337=EDGE_CURVE('',#5984,#5982,#3509,.T.);
#7338=EDGE_CURVE('',#5984,#5985,#3510,.T.);
#7339=EDGE_CURVE('',#5983,#5985,#3511,.T.);
#7340=EDGE_CURVE('',#5986,#5984,#3512,.T.);
#7341=EDGE_CURVE('',#5986,#5987,#3513,.T.);
#7342=EDGE_CURVE('',#5985,#5987,#3514,.T.);
#7343=EDGE_CURVE('',#5988,#5986,#3515,.T.);
#7344=EDGE_CURVE('',#5989,#5988,#3516,.T.);
#7345=EDGE_CURVE('',#5987,#5989,#3517,.T.);
#7346=EDGE_CURVE('',#5990,#5991,#3518,.T.);
#7347=EDGE_CURVE('',#5990,#5992,#3519,.T.);
#7348=EDGE_CURVE('',#5993,#5992,#3520,.T.);
#7349=EDGE_CURVE('',#5991,#5993,#3521,.T.);
#7350=EDGE_CURVE('',#5994,#5990,#3522,.T.);
#7351=EDGE_CURVE('',#5994,#5995,#3523,.T.);
#7352=EDGE_CURVE('',#5992,#5995,#3524,.T.);
#7353=EDGE_CURVE('',#5996,#5994,#3525,.T.);
#7354=EDGE_CURVE('',#5996,#5997,#3526,.T.);
#7355=EDGE_CURVE('',#5995,#5997,#3527,.T.);
#7356=EDGE_CURVE('',#5998,#5996,#3528,.T.);
#7357=EDGE_CURVE('',#5998,#5999,#3529,.T.);
#7358=EDGE_CURVE('',#5997,#5999,#3530,.T.);
#7359=EDGE_CURVE('',#6000,#5998,#3531,.T.);
#7360=EDGE_CURVE('',#6000,#6001,#3532,.T.);
#7361=EDGE_CURVE('',#5999,#6001,#3533,.T.);
#7362=EDGE_CURVE('',#6002,#6000,#3534,.T.);
#7363=EDGE_CURVE('',#6002,#6003,#3535,.T.);
#7364=EDGE_CURVE('',#6001,#6003,#3536,.T.);
#7365=EDGE_CURVE('',#6004,#6002,#3537,.T.);
#7366=EDGE_CURVE('',#6004,#6005,#3538,.T.);
#7367=EDGE_CURVE('',#6003,#6005,#3539,.T.);
#7368=EDGE_CURVE('',#6006,#6004,#3540,.T.);
#7369=EDGE_CURVE('',#6006,#6007,#3541,.T.);
#7370=EDGE_CURVE('',#6005,#6007,#3542,.T.);
#7371=EDGE_CURVE('',#6008,#6006,#3543,.T.);
#7372=EDGE_CURVE('',#6009,#6008,#3544,.T.);
#7373=EDGE_CURVE('',#6007,#6009,#3545,.T.);
#7374=EDGE_CURVE('',#6010,#6011,#3546,.T.);
#7375=EDGE_CURVE('',#6010,#6012,#3547,.T.);
#7376=EDGE_CURVE('',#6013,#6012,#3548,.T.);
#7377=EDGE_CURVE('',#6011,#6013,#3549,.T.);
#7378=EDGE_CURVE('',#6014,#6010,#3550,.T.);
#7379=EDGE_CURVE('',#6014,#6015,#3551,.T.);
#7380=EDGE_CURVE('',#6012,#6015,#3552,.T.);
#7381=EDGE_CURVE('',#6016,#6014,#3553,.T.);
#7382=EDGE_CURVE('',#6016,#6017,#3554,.T.);
#7383=EDGE_CURVE('',#6015,#6017,#3555,.T.);
#7384=EDGE_CURVE('',#6018,#6016,#3556,.T.);
#7385=EDGE_CURVE('',#6018,#6019,#3557,.T.);
#7386=EDGE_CURVE('',#6017,#6019,#3558,.T.);
#7387=EDGE_CURVE('',#6020,#6018,#3559,.T.);
#7388=EDGE_CURVE('',#6020,#6021,#3560,.T.);
#7389=EDGE_CURVE('',#6019,#6021,#3561,.T.);
#7390=EDGE_CURVE('',#6022,#6020,#3562,.T.);
#7391=EDGE_CURVE('',#6022,#6023,#3563,.T.);
#7392=EDGE_CURVE('',#6021,#6023,#3564,.T.);
#7393=EDGE_CURVE('',#6024,#6022,#3565,.T.);
#7394=EDGE_CURVE('',#6024,#6025,#3566,.T.);
#7395=EDGE_CURVE('',#6023,#6025,#3567,.T.);
#7396=EDGE_CURVE('',#6026,#6024,#3568,.T.);
#7397=EDGE_CURVE('',#6026,#6027,#3569,.T.);
#7398=EDGE_CURVE('',#6025,#6027,#3570,.T.);
#7399=EDGE_CURVE('',#6028,#6026,#3571,.T.);
#7400=EDGE_CURVE('',#6029,#6028,#3572,.T.);
#7401=EDGE_CURVE('',#6027,#6029,#3573,.T.);
#7402=EDGE_CURVE('',#6030,#6031,#3574,.T.);
#7403=EDGE_CURVE('',#6030,#6032,#3575,.T.);
#7404=EDGE_CURVE('',#6033,#6032,#3576,.T.);
#7405=EDGE_CURVE('',#6031,#6033,#3577,.T.);
#7406=EDGE_CURVE('',#6034,#6030,#3578,.T.);
#7407=EDGE_CURVE('',#6034,#6035,#3579,.T.);
#7408=EDGE_CURVE('',#6032,#6035,#3580,.T.);
#7409=EDGE_CURVE('',#6036,#6034,#3581,.T.);
#7410=EDGE_CURVE('',#6036,#6037,#3582,.T.);
#7411=EDGE_CURVE('',#6035,#6037,#3583,.T.);
#7412=EDGE_CURVE('',#6038,#6036,#3584,.T.);
#7413=EDGE_CURVE('',#6038,#6039,#3585,.T.);
#7414=EDGE_CURVE('',#6037,#6039,#3586,.T.);
#7415=EDGE_CURVE('',#6040,#6038,#3587,.T.);
#7416=EDGE_CURVE('',#6040,#6041,#3588,.T.);
#7417=EDGE_CURVE('',#6039,#6041,#3589,.T.);
#7418=EDGE_CURVE('',#6042,#6040,#3590,.T.);
#7419=EDGE_CURVE('',#6042,#6043,#3591,.T.);
#7420=EDGE_CURVE('',#6041,#6043,#3592,.T.);
#7421=EDGE_CURVE('',#6044,#6042,#3593,.T.);
#7422=EDGE_CURVE('',#6044,#6045,#3594,.T.);
#7423=EDGE_CURVE('',#6043,#6045,#3595,.T.);
#7424=EDGE_CURVE('',#6046,#6044,#3596,.T.);
#7425=EDGE_CURVE('',#6046,#6047,#3597,.T.);
#7426=EDGE_CURVE('',#6045,#6047,#3598,.T.);
#7427=EDGE_CURVE('',#6048,#6046,#3599,.T.);
#7428=EDGE_CURVE('',#6049,#6048,#3600,.T.);
#7429=EDGE_CURVE('',#6047,#6049,#3601,.T.);
#7430=EDGE_CURVE('',#6050,#6050,#5394,.T.);
#7431=EDGE_CURVE('',#6050,#6051,#3602,.T.);
#7432=EDGE_CURVE('',#6051,#6051,#5395,.T.);
#7433=EDGE_CURVE('',#5988,#6052,#3603,.T.);
#7434=EDGE_CURVE('',#6052,#6053,#3604,.T.);
#7435=EDGE_CURVE('',#5989,#6053,#3605,.T.);
#7436=EDGE_CURVE('',#6054,#5973,#3606,.T.);
#7437=EDGE_CURVE('',#6055,#6054,#3607,.T.);
#7438=EDGE_CURVE('',#6055,#5971,#3608,.T.);
#7439=EDGE_CURVE('',#6008,#6055,#3609,.T.);
#7440=EDGE_CURVE('',#6009,#6054,#3610,.T.);
#7441=EDGE_CURVE('',#6056,#5993,#3611,.T.);
#7442=EDGE_CURVE('',#6057,#6056,#3612,.T.);
#7443=EDGE_CURVE('',#6057,#5991,#3613,.T.);
#7444=EDGE_CURVE('',#6028,#6057,#3614,.T.);
#7445=EDGE_CURVE('',#6029,#6056,#3615,.T.);
#7446=EDGE_CURVE('',#6058,#6013,#3616,.T.);
#7447=EDGE_CURVE('',#6059,#6058,#3617,.T.);
#7448=EDGE_CURVE('',#6059,#6011,#3618,.T.);
#7449=EDGE_CURVE('',#6048,#6059,#3619,.T.);
#7450=EDGE_CURVE('',#6049,#6058,#3620,.T.);
#7451=EDGE_CURVE('',#6053,#6033,#3621,.T.);
#7452=EDGE_CURVE('',#6052,#6031,#3622,.T.);
#7453=EDGE_CURVE('',#6060,#6061,#3623,.T.);
#7454=EDGE_CURVE('',#6061,#6062,#3624,.T.);
#7455=EDGE_CURVE('',#6062,#6063,#3625,.T.);
#7456=EDGE_CURVE('',#6063,#6064,#3626,.T.);
#7457=EDGE_CURVE('',#6064,#6065,#25,.T.);
#7458=EDGE_CURVE('',#6065,#6060,#3627,.T.);
#7459=EDGE_CURVE('',#6066,#6064,#5396,.F.);
#7460=EDGE_CURVE('',#6066,#6067,#3628,.T.);
#7461=EDGE_CURVE('',#6067,#6067,#5397,.T.);
#7462=EDGE_CURVE('',#6068,#6066,#5398,.F.);
#7463=EDGE_CURVE('',#6069,#6068,#26,.T.);
#7464=EDGE_CURVE('',#6065,#6069,#5399,.F.);
#7465=EDGE_CURVE('',#6070,#6063,#3629,.T.);
#7466=EDGE_CURVE('',#6068,#6070,#3630,.T.);
#7467=EDGE_CURVE('',#6071,#6069,#3631,.T.);
#7468=EDGE_CURVE('',#6060,#6071,#3632,.T.);
#7469=EDGE_CURVE('',#6070,#6072,#3633,.T.);
#7470=EDGE_CURVE('',#6072,#6073,#3634,.T.);
#7471=EDGE_CURVE('',#6073,#6071,#3635,.T.);
#7472=EDGE_CURVE('',#6073,#6074,#3636,.T.);
#7473=EDGE_CURVE('',#6075,#6074,#3637,.T.);
#7474=EDGE_CURVE('',#6061,#6075,#3638,.T.);
#7475=EDGE_CURVE('',#6072,#6076,#3639,.T.);
#7476=EDGE_CURVE('',#6074,#6076,#3640,.T.);
#7477=EDGE_CURVE('',#6077,#6075,#3641,.T.);
#7478=EDGE_CURVE('',#6062,#6077,#3642,.T.);
#7479=EDGE_CURVE('',#6076,#6077,#3643,.T.);
#7480=EDGE_CURVE('',#6078,#6078,#5400,.T.);
#7481=EDGE_CURVE('',#6078,#6079,#3644,.T.);
#7482=EDGE_CURVE('',#6079,#6079,#5401,.T.);
#7483=EDGE_CURVE('',#6079,#6080,#3645,.T.);
#7484=EDGE_CURVE('',#6080,#6080,#5402,.T.);
#7485=EDGE_CURVE('',#6081,#6081,#5403,.T.);
#7486=EDGE_CURVE('',#6081,#6082,#3646,.T.);
#7487=EDGE_CURVE('',#6082,#6082,#5404,.T.);
#7488=EDGE_CURVE('',#6083,#6084,#3647,.T.);
#7489=EDGE_CURVE('',#6084,#6085,#3648,.T.);
#7490=EDGE_CURVE('',#6085,#6086,#3649,.T.);
#7491=EDGE_CURVE('',#6083,#6086,#3650,.T.);
#7492=EDGE_CURVE('',#6084,#6087,#3651,.T.);
#7493=EDGE_CURVE('',#6087,#6088,#3652,.T.);
#7494=EDGE_CURVE('',#6088,#6085,#3653,.T.);
#7495=EDGE_CURVE('',#6087,#6089,#3654,.T.);
#7496=EDGE_CURVE('',#6089,#6090,#3655,.T.);
#7497=EDGE_CURVE('',#6090,#6088,#3656,.T.);
#7498=EDGE_CURVE('',#6089,#6091,#3657,.T.);
#7499=EDGE_CURVE('',#6091,#6092,#3658,.T.);
#7500=EDGE_CURVE('',#6092,#6090,#3659,.T.);
#7501=EDGE_CURVE('',#6091,#6093,#3660,.T.);
#7502=EDGE_CURVE('',#6093,#6094,#3661,.T.);
#7503=EDGE_CURVE('',#6094,#6092,#3662,.T.);
#7504=EDGE_CURVE('',#6093,#6083,#3663,.T.);
#7505=EDGE_CURVE('',#6086,#6094,#3664,.T.);
#7506=EDGE_CURVE('',#6095,#6095,#5405,.T.);
#7507=EDGE_CURVE('',#6096,#6096,#5406,.T.);
#7508=EDGE_CURVE('',#6097,#6097,#5407,.T.);
#7509=EDGE_CURVE('',#6097,#6096,#3665,.T.);
#7510=EDGE_CURVE('',#6098,#6098,#5408,.T.);
#7511=EDGE_CURVE('',#6098,#6097,#3666,.T.);
#7512=EDGE_CURVE('',#6099,#6099,#5409,.T.);
#7513=EDGE_CURVE('',#6099,#6098,#3667,.T.);
#7514=EDGE_CURVE('',#6100,#6100,#5410,.T.);
#7515=EDGE_CURVE('',#6101,#6101,#5411,.F.);
#7516=EDGE_CURVE('',#6101,#6100,#3668,.T.);
#7517=EDGE_CURVE('',#6095,#6101,#3669,.T.);
#7518=EDGE_CURVE('',#6102,#6102,#5412,.T.);
#7519=EDGE_CURVE('',#6102,#6103,#3670,.T.);
#7520=EDGE_CURVE('',#6103,#6103,#5413,.T.);
#7521=EDGE_CURVE('',#6104,#6104,#5414,.T.);
#7522=EDGE_CURVE('',#6104,#6105,#3671,.T.);
#7523=EDGE_CURVE('',#6105,#6105,#5415,.T.);
#7524=EDGE_CURVE('',#6106,#6106,#5416,.T.);
#7525=EDGE_CURVE('',#6106,#6107,#3672,.T.);
#7526=EDGE_CURVE('',#6107,#6107,#5417,.T.);
#7527=EDGE_CURVE('',#6108,#6108,#5418,.T.);
#7528=EDGE_CURVE('',#6108,#6109,#3673,.T.);
#7529=EDGE_CURVE('',#6109,#6109,#5419,.T.);
#7530=EDGE_CURVE('',#6110,#6111,#3674,.T.);
#7531=EDGE_CURVE('',#6111,#6112,#3675,.T.);
#7532=EDGE_CURVE('',#6113,#6112,#3676,.T.);
#7533=EDGE_CURVE('',#6110,#6113,#3677,.T.);
#7534=EDGE_CURVE('',#6114,#6110,#3678,.T.);
#7535=EDGE_CURVE('',#6115,#6113,#3679,.T.);
#7536=EDGE_CURVE('',#6114,#6115,#3680,.T.);
#7537=EDGE_CURVE('',#6116,#6114,#3681,.T.);
#7538=EDGE_CURVE('',#6117,#6115,#3682,.T.);
#7539=EDGE_CURVE('',#6116,#6117,#3683,.T.);
#7540=EDGE_CURVE('',#6111,#6116,#3684,.T.);
#7541=EDGE_CURVE('',#6112,#6117,#3685,.T.);
#7542=EDGE_CURVE('',#6118,#6118,#5420,.T.);
#7543=EDGE_CURVE('',#6118,#6119,#3686,.T.);
#7544=EDGE_CURVE('',#6119,#6119,#5421,.T.);
#7545=EDGE_CURVE('',#6120,#6120,#5422,.T.);
#7546=EDGE_CURVE('',#6120,#6121,#3687,.T.);
#7547=EDGE_CURVE('',#6121,#6121,#5423,.T.);
#7548=EDGE_CURVE('',#6122,#6122,#5424,.T.);
#7549=EDGE_CURVE('',#6122,#6123,#3688,.T.);
#7550=EDGE_CURVE('',#6123,#6123,#5425,.T.);
#7551=EDGE_CURVE('',#6124,#6124,#5426,.T.);
#7552=EDGE_CURVE('',#6124,#6125,#3689,.T.);
#7553=EDGE_CURVE('',#6125,#6125,#5427,.T.);
#7554=EDGE_CURVE('',#6126,#6126,#5428,.T.);
#7555=EDGE_CURVE('',#6126,#6127,#3690,.T.);
#7556=EDGE_CURVE('',#6127,#6127,#5429,.T.);
#7557=EDGE_CURVE('',#6128,#6128,#5430,.T.);
#7558=EDGE_CURVE('',#6128,#6129,#3691,.T.);
#7559=EDGE_CURVE('',#6129,#6129,#5431,.T.);
#7560=EDGE_CURVE('',#6130,#6130,#5432,.T.);
#7561=EDGE_CURVE('',#6130,#6131,#3692,.T.);
#7562=EDGE_CURVE('',#6131,#6131,#5433,.T.);
#7563=EDGE_CURVE('',#6132,#6132,#5434,.T.);
#7564=EDGE_CURVE('',#6132,#6133,#3693,.T.);
#7565=EDGE_CURVE('',#6133,#6133,#5435,.T.);
#7566=EDGE_CURVE('',#6134,#6135,#3694,.T.);
#7567=EDGE_CURVE('',#6135,#6136,#3695,.T.);
#7568=EDGE_CURVE('',#6137,#6136,#3696,.T.);
#7569=EDGE_CURVE('',#6134,#6137,#3697,.T.);
#7570=EDGE_CURVE('',#6138,#6134,#3698,.T.);
#7571=EDGE_CURVE('',#6139,#6137,#3699,.T.);
#7572=EDGE_CURVE('',#6138,#6139,#3700,.T.);
#7573=EDGE_CURVE('',#6140,#6138,#3701,.T.);
#7574=EDGE_CURVE('',#6141,#6139,#3702,.T.);
#7575=EDGE_CURVE('',#6140,#6141,#3703,.T.);
#7576=EDGE_CURVE('',#6135,#6140,#3704,.T.);
#7577=EDGE_CURVE('',#6136,#6141,#3705,.T.);
#7578=EDGE_CURVE('',#6142,#6142,#5436,.T.);
#7579=EDGE_CURVE('',#6142,#6143,#3706,.T.);
#7580=EDGE_CURVE('',#6143,#6143,#5437,.T.);
#7581=EDGE_CURVE('',#6144,#6144,#5438,.T.);
#7582=EDGE_CURVE('',#6144,#6145,#3707,.T.);
#7583=EDGE_CURVE('',#6145,#6145,#5439,.T.);
#7584=EDGE_CURVE('',#6146,#6146,#5440,.T.);
#7585=EDGE_CURVE('',#6146,#6147,#3708,.T.);
#7586=EDGE_CURVE('',#6147,#6147,#5441,.T.);
#7587=EDGE_CURVE('',#6148,#6148,#5442,.T.);
#7588=EDGE_CURVE('',#6148,#6149,#3709,.T.);
#7589=EDGE_CURVE('',#6149,#6149,#5443,.T.);
#7590=EDGE_CURVE('',#6150,#6150,#5444,.T.);
#7591=EDGE_CURVE('',#6150,#6151,#3710,.T.);
#7592=EDGE_CURVE('',#6151,#6151,#5445,.T.);
#7593=EDGE_CURVE('',#6152,#6152,#5446,.T.);
#7594=EDGE_CURVE('',#6152,#6153,#3711,.T.);
#7595=EDGE_CURVE('',#6153,#6153,#5447,.T.);
#7596=EDGE_CURVE('',#6154,#6154,#5448,.T.);
#7597=EDGE_CURVE('',#6154,#6155,#3712,.T.);
#7598=EDGE_CURVE('',#6155,#6155,#5449,.T.);
#7599=EDGE_CURVE('',#6156,#6156,#5450,.T.);
#7600=EDGE_CURVE('',#6156,#6157,#3713,.T.);
#7601=EDGE_CURVE('',#6157,#6157,#5451,.T.);
#7602=EDGE_CURVE('',#6158,#6159,#3714,.T.);
#7603=EDGE_CURVE('',#6159,#6160,#3715,.T.);
#7604=EDGE_CURVE('',#6161,#6160,#3716,.T.);
#7605=EDGE_CURVE('',#6158,#6161,#3717,.T.);
#7606=EDGE_CURVE('',#6162,#6158,#3718,.T.);
#7607=EDGE_CURVE('',#6163,#6161,#3719,.T.);
#7608=EDGE_CURVE('',#6162,#6163,#3720,.T.);
#7609=EDGE_CURVE('',#6164,#6162,#3721,.T.);
#7610=EDGE_CURVE('',#6165,#6163,#3722,.T.);
#7611=EDGE_CURVE('',#6164,#6165,#3723,.T.);
#7612=EDGE_CURVE('',#6159,#6164,#3724,.T.);
#7613=EDGE_CURVE('',#6160,#6165,#3725,.T.);
#7614=EDGE_CURVE('',#6166,#6167,#3726,.T.);
#7615=EDGE_CURVE('',#6166,#6167,#5452,.T.);
#7616=EDGE_CURVE('',#6168,#6166,#3727,.T.);
#7617=EDGE_CURVE('',#6169,#6168,#5453,.T.);
#7618=EDGE_CURVE('',#6169,#6170,#3728,.T.);
#7619=EDGE_CURVE('',#6170,#6170,#5454,.T.);
#7620=EDGE_CURVE('',#6171,#6169,#5455,.T.);
#7621=EDGE_CURVE('',#6167,#6171,#3729,.T.);
#7622=EDGE_CURVE('',#6172,#6173,#3730,.T.);
#7623=EDGE_CURVE('',#6172,#6173,#5456,.T.);
#7624=EDGE_CURVE('',#6174,#6172,#3731,.T.);
#7625=EDGE_CURVE('',#6175,#6174,#5457,.T.);
#7626=EDGE_CURVE('',#6175,#6176,#3732,.T.);
#7627=EDGE_CURVE('',#6176,#6176,#5458,.T.);
#7628=EDGE_CURVE('',#6177,#6175,#5459,.T.);
#7629=EDGE_CURVE('',#6173,#6177,#3733,.T.);
#7630=EDGE_CURVE('',#6178,#6179,#3734,.T.);
#7631=EDGE_CURVE('',#6178,#6179,#5460,.T.);
#7632=EDGE_CURVE('',#6180,#6178,#3735,.T.);
#7633=EDGE_CURVE('',#6181,#6180,#5461,.T.);
#7634=EDGE_CURVE('',#6181,#6182,#3736,.T.);
#7635=EDGE_CURVE('',#6182,#6182,#5462,.T.);
#7636=EDGE_CURVE('',#6183,#6181,#5463,.T.);
#7637=EDGE_CURVE('',#6179,#6183,#3737,.T.);
#7638=EDGE_CURVE('',#6184,#6185,#3738,.T.);
#7639=EDGE_CURVE('',#6184,#6185,#5464,.T.);
#7640=EDGE_CURVE('',#6186,#6184,#3739,.T.);
#7641=EDGE_CURVE('',#6187,#6186,#5465,.T.);
#7642=EDGE_CURVE('',#6187,#6188,#3740,.T.);
#7643=EDGE_CURVE('',#6188,#6188,#5466,.T.);
#7644=EDGE_CURVE('',#6189,#6187,#5467,.T.);
#7645=EDGE_CURVE('',#6185,#6189,#3741,.T.);
#7646=EDGE_CURVE('',#6171,#6180,#3742,.T.);
#7647=EDGE_CURVE('',#6183,#6190,#3743,.T.);
#7648=EDGE_CURVE('',#6191,#6190,#3744,.T.);
#7649=EDGE_CURVE('',#6191,#6192,#3745,.T.);
#7650=EDGE_CURVE('',#6193,#6192,#3746,.T.);
#7651=EDGE_CURVE('',#6193,#6168,#3747,.T.);
#7652=EDGE_CURVE('',#6177,#6186,#3748,.T.);
#7653=EDGE_CURVE('',#6189,#6194,#3749,.T.);
#7654=EDGE_CURVE('',#6195,#6194,#3750,.T.);
#7655=EDGE_CURVE('',#6196,#6195,#3751,.T.);
#7656=EDGE_CURVE('',#6197,#6196,#3752,.T.);
#7657=EDGE_CURVE('',#6197,#6174,#3753,.T.);
#7658=EDGE_CURVE('',#6190,#6198,#3754,.T.);
#7659=EDGE_CURVE('',#6198,#6199,#3755,.T.);
#7660=EDGE_CURVE('',#6199,#6200,#3756,.T.);
#7661=EDGE_CURVE('',#6200,#6201,#3757,.T.);
#7662=EDGE_CURVE('',#6201,#6197,#3758,.T.);
#7663=EDGE_CURVE('',#6196,#6202,#3759,.T.);
#7664=EDGE_CURVE('',#6202,#6203,#3760,.T.);
#7665=EDGE_CURVE('',#6203,#6204,#3761,.T.);
#7666=EDGE_CURVE('',#6204,#6205,#3762,.T.);
#7667=EDGE_CURVE('',#6205,#6191,#3763,.T.);
#7668=EDGE_CURVE('',#6206,#6193,#3764,.T.);
#7669=EDGE_CURVE('',#6198,#6206,#3765,.T.);
#7670=EDGE_CURVE('',#6207,#6206,#3766,.T.);
#7671=EDGE_CURVE('',#6199,#6207,#3767,.T.);
#7672=EDGE_CURVE('',#6208,#6207,#3768,.T.);
#7673=EDGE_CURVE('',#6200,#6208,#3769,.T.);
#7674=EDGE_CURVE('',#6209,#6208,#3770,.T.);
#7675=EDGE_CURVE('',#6201,#6209,#3771,.T.);
#7676=EDGE_CURVE('',#6194,#6209,#3772,.T.);
#7677=EDGE_CURVE('',#6210,#6195,#3773,.T.);
#7678=EDGE_CURVE('',#6202,#6210,#3774,.T.);
#7679=EDGE_CURVE('',#6211,#6210,#3775,.T.);
#7680=EDGE_CURVE('',#6203,#6211,#3776,.T.);
#7681=EDGE_CURVE('',#6212,#6211,#3777,.T.);
#7682=EDGE_CURVE('',#6204,#6212,#3778,.T.);
#7683=EDGE_CURVE('',#6213,#6212,#3779,.T.);
#7684=EDGE_CURVE('',#6205,#6213,#3780,.T.);
#7685=EDGE_CURVE('',#6192,#6213,#3781,.T.);
#7686=EDGE_CURVE('',#6214,#6215,#3782,.T.);
#7687=EDGE_CURVE('',#6215,#6216,#3783,.T.);
#7688=EDGE_CURVE('',#6217,#6216,#3784,.T.);
#7689=EDGE_CURVE('',#6214,#6217,#3785,.T.);
#7690=EDGE_CURVE('',#6218,#6214,#3786,.T.);
#7691=EDGE_CURVE('',#6219,#6217,#3787,.T.);
#7692=EDGE_CURVE('',#6218,#6219,#3788,.T.);
#7693=EDGE_CURVE('',#6220,#6218,#3789,.T.);
#7694=EDGE_CURVE('',#6221,#6219,#3790,.T.);
#7695=EDGE_CURVE('',#6220,#6221,#3791,.T.);
#7696=EDGE_CURVE('',#6222,#6220,#3792,.T.);
#7697=EDGE_CURVE('',#6223,#6221,#3793,.T.);
#7698=EDGE_CURVE('',#6222,#6223,#3794,.T.);
#7699=EDGE_CURVE('',#6224,#6222,#3795,.T.);
#7700=EDGE_CURVE('',#6225,#6223,#3796,.T.);
#7701=EDGE_CURVE('',#6224,#6225,#3797,.T.);
#7702=EDGE_CURVE('',#6226,#6224,#3798,.T.);
#7703=EDGE_CURVE('',#6227,#6225,#3799,.T.);
#7704=EDGE_CURVE('',#6226,#6227,#3800,.T.);
#7705=EDGE_CURVE('',#6228,#6226,#3801,.T.);
#7706=EDGE_CURVE('',#6229,#6227,#3802,.T.);
#7707=EDGE_CURVE('',#6228,#6229,#3803,.T.);
#7708=EDGE_CURVE('',#6215,#6228,#3804,.T.);
#7709=EDGE_CURVE('',#6216,#6229,#3805,.T.);
#7710=EDGE_CURVE('',#6230,#6231,#3806,.T.);
#7711=EDGE_CURVE('',#6230,#6232,#3807,.T.);
#7712=EDGE_CURVE('',#6233,#6232,#3808,.T.);
#7713=EDGE_CURVE('',#6231,#6233,#3809,.T.);
#7714=EDGE_CURVE('',#6231,#6234,#3810,.T.);
#7715=EDGE_CURVE('',#6235,#6233,#3811,.T.);
#7716=EDGE_CURVE('',#6234,#6235,#3812,.T.);
#7717=EDGE_CURVE('',#6234,#6236,#3813,.T.);
#7718=EDGE_CURVE('',#6237,#6235,#3814,.T.);
#7719=EDGE_CURVE('',#6236,#6237,#3815,.T.);
#7720=EDGE_CURVE('',#6236,#6238,#3816,.T.);
#7721=EDGE_CURVE('',#6239,#6237,#3817,.T.);
#7722=EDGE_CURVE('',#6238,#6239,#3818,.T.);
#7723=EDGE_CURVE('',#6238,#6240,#3819,.T.);
#7724=EDGE_CURVE('',#6241,#6239,#3820,.T.);
#7725=EDGE_CURVE('',#6240,#6241,#3821,.T.);
#7726=EDGE_CURVE('',#6240,#6242,#3822,.T.);
#7727=EDGE_CURVE('',#6243,#6241,#3823,.T.);
#7728=EDGE_CURVE('',#6242,#6243,#3824,.T.);
#7729=EDGE_CURVE('',#6242,#6244,#3825,.T.);
#7730=EDGE_CURVE('',#6245,#6243,#3826,.T.);
#7731=EDGE_CURVE('',#6244,#6245,#3827,.T.);
#7732=EDGE_CURVE('',#6244,#6230,#3828,.T.);
#7733=EDGE_CURVE('',#6232,#6245,#3829,.T.);
#7734=EDGE_CURVE('',#6246,#6246,#5468,.T.);
#7735=EDGE_CURVE('',#6246,#6247,#3830,.T.);
#7736=EDGE_CURVE('',#6247,#6247,#5469,.T.);
#7737=EDGE_CURVE('',#6247,#6248,#3831,.T.);
#7738=EDGE_CURVE('',#6248,#6248,#5470,.T.);
#7739=EDGE_CURVE('',#6249,#6249,#5471,.T.);
#7740=EDGE_CURVE('',#6249,#6250,#3832,.T.);
#7741=EDGE_CURVE('',#6250,#6250,#5472,.T.);
#7742=EDGE_CURVE('',#6251,#6252,#3833,.T.);
#7743=EDGE_CURVE('',#6252,#6253,#3834,.T.);
#7744=EDGE_CURVE('',#6253,#6254,#3835,.T.);
#7745=EDGE_CURVE('',#6251,#6254,#3836,.T.);
#7746=EDGE_CURVE('',#6252,#6255,#3837,.T.);
#7747=EDGE_CURVE('',#6255,#6256,#3838,.T.);
#7748=EDGE_CURVE('',#6256,#6253,#3839,.T.);
#7749=EDGE_CURVE('',#6255,#6257,#3840,.T.);
#7750=EDGE_CURVE('',#6257,#6258,#3841,.T.);
#7751=EDGE_CURVE('',#6258,#6256,#3842,.T.);
#7752=EDGE_CURVE('',#6257,#6259,#3843,.T.);
#7753=EDGE_CURVE('',#6259,#6260,#3844,.T.);
#7754=EDGE_CURVE('',#6260,#6258,#3845,.T.);
#7755=EDGE_CURVE('',#6259,#6261,#3846,.T.);
#7756=EDGE_CURVE('',#6261,#6262,#3847,.T.);
#7757=EDGE_CURVE('',#6262,#6260,#3848,.T.);
#7758=EDGE_CURVE('',#6261,#6251,#3849,.T.);
#7759=EDGE_CURVE('',#6254,#6262,#3850,.T.);
#7760=EDGE_CURVE('',#6263,#6263,#5473,.T.);
#7761=EDGE_CURVE('',#6264,#6264,#5474,.T.);
#7762=EDGE_CURVE('',#6263,#6265,#3851,.T.);
#7763=EDGE_CURVE('',#6265,#6265,#5475,.T.);
#7764=EDGE_CURVE('',#6266,#6266,#5476,.T.);
#7765=EDGE_CURVE('',#6267,#6267,#5477,.T.);
#7766=EDGE_CURVE('',#6267,#6266,#3852,.T.);
#7767=EDGE_CURVE('',#6268,#6268,#5478,.T.);
#7768=EDGE_CURVE('',#6268,#6267,#3853,.T.);
#7769=EDGE_CURVE('',#6269,#6269,#5479,.T.);
#7770=EDGE_CURVE('',#6269,#6268,#3854,.T.);
#7771=EDGE_CURVE('',#6270,#6270,#5480,.T.);
#7772=EDGE_CURVE('',#6271,#6271,#5481,.F.);
#7773=EDGE_CURVE('',#6271,#6270,#3855,.T.);
#7774=EDGE_CURVE('',#6264,#6271,#3856,.T.);
#7775=EDGE_CURVE('',#6272,#6273,#3857,.T.);
#7776=EDGE_CURVE('',#6273,#6274,#435,.T.);
#7777=EDGE_CURVE('',#6274,#6275,#5482,.F.);
#7778=EDGE_CURVE('',#6275,#6272,#436,.T.);
#7779=EDGE_CURVE('',#6276,#6277,#3858,.T.);
#7780=EDGE_CURVE('',#6277,#6273,#437,.T.);
#7781=EDGE_CURVE('',#6272,#6276,#438,.T.);
#7782=EDGE_CURVE('',#6278,#6279,#3859,.T.);
#7783=EDGE_CURVE('',#6279,#6277,#439,.T.);
#7784=EDGE_CURVE('',#6276,#6278,#440,.T.);
#7785=EDGE_CURVE('',#6280,#6281,#3860,.T.);
#7786=EDGE_CURVE('',#6281,#6279,#441,.T.);
#7787=EDGE_CURVE('',#6278,#6280,#442,.T.);
#7788=EDGE_CURVE('',#6282,#6283,#3861,.T.);
#7789=EDGE_CURVE('',#6283,#6281,#443,.T.);
#7790=EDGE_CURVE('',#6280,#6282,#444,.T.);
#7791=EDGE_CURVE('',#6284,#6285,#3862,.T.);
#7792=EDGE_CURVE('',#6285,#6283,#445,.T.);
#7793=EDGE_CURVE('',#6282,#6284,#446,.T.);
#7794=EDGE_CURVE('',#6286,#6287,#3863,.T.);
#7795=EDGE_CURVE('',#6287,#6285,#447,.T.);
#7796=EDGE_CURVE('',#6284,#6286,#448,.T.);
#7797=EDGE_CURVE('',#6288,#6289,#3864,.T.);
#7798=EDGE_CURVE('',#6289,#6287,#449,.T.);
#7799=EDGE_CURVE('',#6286,#6288,#450,.T.);
#7800=EDGE_CURVE('',#6290,#6291,#3865,.T.);
#7801=EDGE_CURVE('',#6292,#6290,#5483,.F.);
#7802=EDGE_CURVE('',#6292,#6291,#451,.T.);
#7803=EDGE_CURVE('',#6293,#6294,#3866,.T.);
#7804=EDGE_CURVE('',#6294,#6295,#452,.T.);
#7805=EDGE_CURVE('',#6296,#6295,#5484,.T.);
#7806=EDGE_CURVE('',#6293,#6296,#453,.T.);
#7807=EDGE_CURVE('',#6297,#6298,#3867,.T.);
#7808=EDGE_CURVE('',#6298,#6294,#454,.T.);
#7809=EDGE_CURVE('',#6297,#6293,#455,.T.);
#7810=EDGE_CURVE('',#6299,#6300,#3868,.T.);
#7811=EDGE_CURVE('',#6300,#6298,#456,.T.);
#7812=EDGE_CURVE('',#6299,#6297,#457,.T.);
#7813=EDGE_CURVE('',#6301,#6302,#3869,.T.);
#7814=EDGE_CURVE('',#6302,#6300,#458,.T.);
#7815=EDGE_CURVE('',#6301,#6299,#459,.T.);
#7816=EDGE_CURVE('',#6303,#6304,#3870,.T.);
#7817=EDGE_CURVE('',#6304,#6302,#460,.T.);
#7818=EDGE_CURVE('',#6303,#6301,#461,.T.);
#7819=EDGE_CURVE('',#6305,#6306,#3871,.T.);
#7820=EDGE_CURVE('',#6306,#6304,#462,.T.);
#7821=EDGE_CURVE('',#6305,#6303,#463,.T.);
#7822=EDGE_CURVE('',#6307,#6308,#3872,.T.);
#7823=EDGE_CURVE('',#6308,#6306,#464,.T.);
#7824=EDGE_CURVE('',#6307,#6305,#465,.T.);
#7825=EDGE_CURVE('',#6309,#6310,#3873,.T.);
#7826=EDGE_CURVE('',#6310,#6308,#466,.T.);
#7827=EDGE_CURVE('',#6309,#6307,#467,.T.);
#7828=EDGE_CURVE('',#6311,#6312,#3874,.T.);
#7829=EDGE_CURVE('',#6313,#6311,#468,.T.);
#7830=EDGE_CURVE('',#6314,#6313,#5485,.T.);
#7831=EDGE_CURVE('',#6314,#6312,#469,.T.);
#7832=EDGE_CURVE('',#6312,#6310,#470,.T.);
#7833=EDGE_CURVE('',#6311,#6309,#471,.T.);
#7834=EDGE_CURVE('',#6295,#6292,#472,.T.);
#7835=EDGE_CURVE('',#6274,#6314,#473,.T.);
#7836=EDGE_CURVE('',#6291,#6289,#474,.T.);
#7837=EDGE_CURVE('',#6315,#6296,#475,.T.);
#7838=EDGE_CURVE('',#6288,#6315,#476,.T.);
#7839=EDGE_CURVE('',#6313,#6275,#477,.T.);
#7840=EDGE_CURVE('',#6316,#6317,#3875,.T.);
#7841=EDGE_CURVE('',#6317,#6316,#5486,.T.);
#7842=EDGE_CURVE('',#6290,#6315,#5487,.F.);
#7843=EDGE_CURVE('',#6318,#6318,#5488,.T.);
#7844=EDGE_CURVE('',#6319,#6319,#5489,.T.);
#7845=EDGE_CURVE('',#6320,#6320,#5490,.T.);
#7846=EDGE_CURVE('',#6321,#6321,#5491,.T.);
#7847=EDGE_CURVE('',#6321,#6320,#3876,.T.);
#7848=EDGE_CURVE('',#6322,#6322,#5492,.T.);
#7849=EDGE_CURVE('',#6322,#6319,#3877,.T.);
#7850=EDGE_CURVE('',#6323,#6323,#5493,.T.);
#7851=EDGE_CURVE('',#6323,#6318,#3878,.T.);
#7852=EDGE_CURVE('',#6324,#6325,#3879,.T.);
#7853=EDGE_CURVE('',#6317,#6324,#3880,.T.);
#7854=EDGE_CURVE('',#6325,#6316,#3881,.T.);
#7855=EDGE_CURVE('',#6324,#6325,#5494,.T.);
#7856=EDGE_CURVE('',#6326,#6326,#5495,.T.);
#7857=EDGE_CURVE('',#6326,#6327,#3882,.T.);
#7858=EDGE_CURVE('',#6327,#6327,#5496,.T.);
#7859=EDGE_CURVE('',#6328,#6328,#5497,.T.);
#7860=EDGE_CURVE('',#6329,#6329,#5498,.T.);
#7861=EDGE_CURVE('',#6329,#6328,#3883,.T.);
#7862=EDGE_CURVE('',#6330,#6330,#5499,.T.);
#7863=EDGE_CURVE('',#6330,#6329,#3884,.T.);
#7864=EDGE_CURVE('',#6331,#6331,#5500,.T.);
#7865=EDGE_CURVE('',#6331,#6330,#3885,.T.);
#7866=EDGE_CURVE('',#6332,#6332,#5501,.T.);
#7867=EDGE_CURVE('',#6333,#6333,#5502,.F.);
#7868=EDGE_CURVE('',#6333,#6332,#3886,.T.);
#7869=EDGE_CURVE('',#6334,#6334,#5503,.F.);
#7870=EDGE_CURVE('',#6334,#6333,#3887,.T.);
#7871=EDGE_CURVE('',#6335,#6335,#5504,.T.);
#7872=EDGE_CURVE('',#6335,#6334,#3888,.T.);
#7873=EDGE_CURVE('',#6336,#6337,#3889,.T.);
#7874=EDGE_CURVE('',#6337,#6338,#3890,.T.);
#7875=EDGE_CURVE('',#6338,#6339,#3891,.T.);
#7876=EDGE_CURVE('',#6336,#6339,#3892,.T.);
#7877=EDGE_CURVE('',#6337,#6340,#3893,.T.);
#7878=EDGE_CURVE('',#6340,#6341,#3894,.T.);
#7879=EDGE_CURVE('',#6341,#6338,#3895,.T.);
#7880=EDGE_CURVE('',#6340,#6342,#3896,.T.);
#7881=EDGE_CURVE('',#6342,#6343,#3897,.T.);
#7882=EDGE_CURVE('',#6343,#6341,#3898,.T.);
#7883=EDGE_CURVE('',#6342,#6344,#3899,.T.);
#7884=EDGE_CURVE('',#6344,#6345,#3900,.T.);
#7885=EDGE_CURVE('',#6345,#6343,#3901,.T.);
#7886=EDGE_CURVE('',#6344,#6346,#3902,.T.);
#7887=EDGE_CURVE('',#6346,#6347,#3903,.T.);
#7888=EDGE_CURVE('',#6347,#6345,#3904,.T.);
#7889=EDGE_CURVE('',#6346,#6336,#3905,.T.);
#7890=EDGE_CURVE('',#6339,#6347,#3906,.T.);
#7891=EDGE_CURVE('',#6348,#6348,#5505,.T.);
#7892=EDGE_CURVE('',#6349,#6349,#5506,.T.);
#7893=EDGE_CURVE('',#6349,#6348,#3907,.T.);
#7894=EDGE_CURVE('',#6350,#6350,#5507,.T.);
#7895=EDGE_CURVE('',#6350,#6349,#3908,.T.);
#7896=EDGE_CURVE('',#6351,#6351,#5508,.T.);
#7897=EDGE_CURVE('',#6351,#6350,#3909,.T.);
#7898=EDGE_CURVE('',#6352,#6352,#5509,.T.);
#7899=EDGE_CURVE('',#6353,#6353,#5510,.F.);
#7900=EDGE_CURVE('',#6353,#6352,#3910,.T.);
#7901=EDGE_CURVE('',#6354,#6354,#5511,.F.);
#7902=EDGE_CURVE('',#6354,#6353,#3911,.T.);
#7903=EDGE_CURVE('',#6355,#6355,#5512,.T.);
#7904=EDGE_CURVE('',#6355,#6354,#3912,.T.);
#7905=EDGE_CURVE('',#6356,#6357,#3913,.T.);
#7906=EDGE_CURVE('',#6357,#6358,#3914,.T.);
#7907=EDGE_CURVE('',#6358,#6359,#3915,.T.);
#7908=EDGE_CURVE('',#6356,#6359,#3916,.T.);
#7909=EDGE_CURVE('',#6357,#6360,#3917,.T.);
#7910=EDGE_CURVE('',#6360,#6361,#3918,.T.);
#7911=EDGE_CURVE('',#6361,#6358,#3919,.T.);
#7912=EDGE_CURVE('',#6360,#6362,#3920,.T.);
#7913=EDGE_CURVE('',#6362,#6363,#3921,.T.);
#7914=EDGE_CURVE('',#6363,#6361,#3922,.T.);
#7915=EDGE_CURVE('',#6362,#6364,#3923,.T.);
#7916=EDGE_CURVE('',#6364,#6365,#3924,.T.);
#7917=EDGE_CURVE('',#6365,#6363,#3925,.T.);
#7918=EDGE_CURVE('',#6364,#6366,#3926,.T.);
#7919=EDGE_CURVE('',#6366,#6367,#3927,.T.);
#7920=EDGE_CURVE('',#6367,#6365,#3928,.T.);
#7921=EDGE_CURVE('',#6366,#6356,#3929,.T.);
#7922=EDGE_CURVE('',#6359,#6367,#3930,.T.);
#7923=EDGE_CURVE('',#6368,#6369,#3931,.T.);
#7924=EDGE_CURVE('',#6368,#6370,#478,.T.);
#7925=EDGE_CURVE('',#6370,#6371,#5513,.F.);
#7926=EDGE_CURVE('',#6371,#6369,#479,.T.);
#7927=EDGE_CURVE('',#6372,#6373,#3932,.T.);
#7928=EDGE_CURVE('',#6372,#6368,#480,.T.);
#7929=EDGE_CURVE('',#6369,#6373,#481,.T.);
#7930=EDGE_CURVE('',#6374,#6375,#3933,.T.);
#7931=EDGE_CURVE('',#6374,#6372,#482,.T.);
#7932=EDGE_CURVE('',#6373,#6375,#483,.T.);
#7933=EDGE_CURVE('',#6376,#6377,#3934,.T.);
#7934=EDGE_CURVE('',#6376,#6374,#484,.T.);
#7935=EDGE_CURVE('',#6375,#6377,#485,.T.);
#7936=EDGE_CURVE('',#6378,#6379,#3935,.T.);
#7937=EDGE_CURVE('',#6378,#6376,#486,.T.);
#7938=EDGE_CURVE('',#6377,#6379,#487,.T.);
#7939=EDGE_CURVE('',#6380,#6381,#3936,.T.);
#7940=EDGE_CURVE('',#6380,#6378,#488,.T.);
#7941=EDGE_CURVE('',#6379,#6381,#489,.T.);
#7942=EDGE_CURVE('',#6382,#6383,#3937,.T.);
#7943=EDGE_CURVE('',#6382,#6380,#490,.T.);
#7944=EDGE_CURVE('',#6381,#6383,#491,.T.);
#7945=EDGE_CURVE('',#6384,#6385,#3938,.T.);
#7946=EDGE_CURVE('',#6384,#6382,#492,.T.);
#7947=EDGE_CURVE('',#6383,#6385,#493,.T.);
#7948=EDGE_CURVE('',#6386,#6387,#3939,.T.);
#7949=EDGE_CURVE('',#6386,#6384,#494,.T.);
#7950=EDGE_CURVE('',#6385,#6387,#495,.T.);
#7951=EDGE_CURVE('',#6388,#6389,#3940,.T.);
#7952=EDGE_CURVE('',#6388,#6386,#496,.T.);
#7953=EDGE_CURVE('',#6387,#6389,#497,.T.);
#7954=EDGE_CURVE('',#6390,#6391,#3941,.T.);
#7955=EDGE_CURVE('',#6390,#6388,#498,.T.);
#7956=EDGE_CURVE('',#6389,#6391,#499,.T.);
#7957=EDGE_CURVE('',#6392,#6393,#3942,.T.);
#7958=EDGE_CURVE('',#6392,#6390,#500,.T.);
#7959=EDGE_CURVE('',#6391,#6393,#501,.T.);
#7960=EDGE_CURVE('',#6394,#6395,#3943,.T.);
#7961=EDGE_CURVE('',#6394,#6392,#502,.T.);
#7962=EDGE_CURVE('',#6393,#6395,#503,.T.);
#7963=EDGE_CURVE('',#6396,#6397,#3944,.T.);
#7964=EDGE_CURVE('',#6396,#6394,#504,.T.);
#7965=EDGE_CURVE('',#6395,#6397,#505,.T.);
#7966=EDGE_CURVE('',#6398,#6399,#3945,.T.);
#7967=EDGE_CURVE('',#6398,#6396,#506,.T.);
#7968=EDGE_CURVE('',#6397,#6399,#507,.T.);
#7969=EDGE_CURVE('',#6400,#6401,#3946,.T.);
#7970=EDGE_CURVE('',#6400,#6398,#508,.T.);
#7971=EDGE_CURVE('',#6399,#6401,#509,.T.);
#7972=EDGE_CURVE('',#6402,#6403,#3947,.T.);
#7973=EDGE_CURVE('',#6402,#6400,#510,.T.);
#7974=EDGE_CURVE('',#6401,#6403,#511,.T.);
#7975=EDGE_CURVE('',#6404,#6405,#3948,.T.);
#7976=EDGE_CURVE('',#6404,#6402,#512,.T.);
#7977=EDGE_CURVE('',#6403,#6405,#513,.T.);
#7978=EDGE_CURVE('',#6406,#6407,#3949,.T.);
#7979=EDGE_CURVE('',#6406,#6404,#514,.T.);
#7980=EDGE_CURVE('',#6405,#6407,#515,.T.);
#7981=EDGE_CURVE('',#6408,#6409,#3950,.T.);
#7982=EDGE_CURVE('',#6408,#6406,#516,.T.);
#7983=EDGE_CURVE('',#6407,#6409,#517,.T.);
#7984=EDGE_CURVE('',#6410,#6411,#3951,.T.);
#7985=EDGE_CURVE('',#6410,#6408,#518,.T.);
#7986=EDGE_CURVE('',#6409,#6411,#519,.T.);
#7987=EDGE_CURVE('',#6412,#6413,#3952,.T.);
#7988=EDGE_CURVE('',#6412,#6410,#520,.T.);
#7989=EDGE_CURVE('',#6411,#6413,#521,.T.);
#7990=EDGE_CURVE('',#6414,#6415,#3953,.T.);
#7991=EDGE_CURVE('',#6414,#6412,#522,.T.);
#7992=EDGE_CURVE('',#6413,#6415,#523,.T.);
#7993=EDGE_CURVE('',#6416,#6417,#3954,.T.);
#7994=EDGE_CURVE('',#6416,#6414,#524,.T.);
#7995=EDGE_CURVE('',#6415,#6417,#525,.T.);
#7996=EDGE_CURVE('',#6418,#6419,#3955,.T.);
#7997=EDGE_CURVE('',#6418,#6416,#526,.T.);
#7998=EDGE_CURVE('',#6417,#6419,#527,.T.);
#7999=EDGE_CURVE('',#6420,#6421,#3956,.T.);
#8000=EDGE_CURVE('',#6420,#6418,#528,.T.);
#8001=EDGE_CURVE('',#6419,#6421,#529,.T.);
#8002=EDGE_CURVE('',#6422,#6423,#3957,.T.);
#8003=EDGE_CURVE('',#6422,#6420,#530,.T.);
#8004=EDGE_CURVE('',#6421,#6423,#531,.T.);
#8005=EDGE_CURVE('',#6424,#6425,#3958,.T.);
#8006=EDGE_CURVE('',#6424,#6422,#532,.T.);
#8007=EDGE_CURVE('',#6423,#6425,#533,.T.);
#8008=EDGE_CURVE('',#6426,#6427,#3959,.T.);
#8009=EDGE_CURVE('',#6426,#6424,#534,.T.);
#8010=EDGE_CURVE('',#6425,#6427,#535,.T.);
#8011=EDGE_CURVE('',#6428,#6429,#3960,.T.);
#8012=EDGE_CURVE('',#6428,#6426,#536,.T.);
#8013=EDGE_CURVE('',#6427,#6429,#537,.T.);
#8014=EDGE_CURVE('',#6430,#6431,#3961,.T.);
#8015=EDGE_CURVE('',#6430,#6428,#538,.T.);
#8016=EDGE_CURVE('',#6429,#6431,#539,.T.);
#8017=EDGE_CURVE('',#6432,#6433,#3962,.T.);
#8018=EDGE_CURVE('',#6432,#6430,#540,.T.);
#8019=EDGE_CURVE('',#6431,#6433,#541,.T.);
#8020=EDGE_CURVE('',#6434,#6435,#3963,.T.);
#8021=EDGE_CURVE('',#6434,#6432,#542,.T.);
#8022=EDGE_CURVE('',#6433,#6435,#543,.T.);
#8023=EDGE_CURVE('',#6436,#6437,#3964,.T.);
#8024=EDGE_CURVE('',#6436,#6434,#544,.T.);
#8025=EDGE_CURVE('',#6435,#6437,#545,.T.);
#8026=EDGE_CURVE('',#6438,#6439,#3965,.T.);
#8027=EDGE_CURVE('',#6438,#6436,#546,.T.);
#8028=EDGE_CURVE('',#6437,#6439,#547,.T.);
#8029=EDGE_CURVE('',#6440,#6441,#3966,.T.);
#8030=EDGE_CURVE('',#6440,#6438,#548,.T.);
#8031=EDGE_CURVE('',#6439,#6441,#549,.T.);
#8032=EDGE_CURVE('',#6442,#6443,#3967,.T.);
#8033=EDGE_CURVE('',#6442,#6440,#550,.T.);
#8034=EDGE_CURVE('',#6441,#6443,#551,.T.);
#8035=EDGE_CURVE('',#6444,#6445,#3968,.T.);
#8036=EDGE_CURVE('',#6444,#6442,#552,.T.);
#8037=EDGE_CURVE('',#6443,#6445,#553,.T.);
#8038=EDGE_CURVE('',#6446,#6447,#3969,.T.);
#8039=EDGE_CURVE('',#6446,#6444,#554,.T.);
#8040=EDGE_CURVE('',#6445,#6447,#555,.T.);
#8041=EDGE_CURVE('',#6448,#6449,#3970,.T.);
#8042=EDGE_CURVE('',#6448,#6446,#556,.T.);
#8043=EDGE_CURVE('',#6447,#6449,#557,.T.);
#8044=EDGE_CURVE('',#6450,#6451,#3971,.T.);
#8045=EDGE_CURVE('',#6450,#6448,#558,.T.);
#8046=EDGE_CURVE('',#6449,#6451,#559,.T.);
#8047=EDGE_CURVE('',#6452,#6453,#3972,.T.);
#8048=EDGE_CURVE('',#6452,#6450,#560,.T.);
#8049=EDGE_CURVE('',#6451,#6453,#561,.T.);
#8050=EDGE_CURVE('',#6454,#6455,#3973,.T.);
#8051=EDGE_CURVE('',#6454,#6452,#562,.T.);
#8052=EDGE_CURVE('',#6453,#6455,#563,.T.);
#8053=EDGE_CURVE('',#6456,#6457,#3974,.T.);
#8054=EDGE_CURVE('',#6456,#6454,#564,.T.);
#8055=EDGE_CURVE('',#6455,#6457,#565,.T.);
#8056=EDGE_CURVE('',#6458,#6459,#3975,.T.);
#8057=EDGE_CURVE('',#6458,#6456,#566,.T.);
#8058=EDGE_CURVE('',#6457,#6459,#567,.T.);
#8059=EDGE_CURVE('',#6460,#6461,#3976,.T.);
#8060=EDGE_CURVE('',#6460,#6458,#568,.T.);
#8061=EDGE_CURVE('',#6459,#6461,#569,.T.);
#8062=EDGE_CURVE('',#6462,#6463,#3977,.T.);
#8063=EDGE_CURVE('',#6462,#6460,#570,.T.);
#8064=EDGE_CURVE('',#6461,#6463,#571,.T.);
#8065=EDGE_CURVE('',#6464,#6465,#3978,.T.);
#8066=EDGE_CURVE('',#6464,#6462,#572,.T.);
#8067=EDGE_CURVE('',#6463,#6465,#573,.T.);
#8068=EDGE_CURVE('',#6466,#6467,#3979,.T.);
#8069=EDGE_CURVE('',#6466,#6464,#574,.T.);
#8070=EDGE_CURVE('',#6465,#6467,#575,.T.);
#8071=EDGE_CURVE('',#6468,#6469,#3980,.T.);
#8072=EDGE_CURVE('',#6468,#6466,#576,.T.);
#8073=EDGE_CURVE('',#6467,#6469,#577,.T.);
#8074=EDGE_CURVE('',#6470,#6471,#3981,.T.);
#8075=EDGE_CURVE('',#6470,#6468,#578,.T.);
#8076=EDGE_CURVE('',#6469,#6471,#579,.T.);
#8077=EDGE_CURVE('',#6472,#6473,#3982,.T.);
#8078=EDGE_CURVE('',#6472,#6470,#580,.T.);
#8079=EDGE_CURVE('',#6471,#6473,#581,.T.);
#8080=EDGE_CURVE('',#6474,#6475,#3983,.T.);
#8081=EDGE_CURVE('',#6474,#6472,#582,.T.);
#8082=EDGE_CURVE('',#6473,#6475,#583,.T.);
#8083=EDGE_CURVE('',#6476,#6477,#3984,.T.);
#8084=EDGE_CURVE('',#6476,#6474,#584,.T.);
#8085=EDGE_CURVE('',#6475,#6477,#585,.T.);
#8086=EDGE_CURVE('',#6478,#6479,#3985,.T.);
#8087=EDGE_CURVE('',#6478,#6476,#586,.T.);
#8088=EDGE_CURVE('',#6477,#6479,#587,.T.);
#8089=EDGE_CURVE('',#6480,#6481,#3986,.T.);
#8090=EDGE_CURVE('',#6480,#6478,#588,.T.);
#8091=EDGE_CURVE('',#6479,#6481,#589,.T.);
#8092=EDGE_CURVE('',#6482,#6483,#3987,.T.);
#8093=EDGE_CURVE('',#6482,#6480,#590,.T.);
#8094=EDGE_CURVE('',#6481,#6483,#591,.T.);
#8095=EDGE_CURVE('',#6484,#6485,#3988,.T.);
#8096=EDGE_CURVE('',#6484,#6482,#592,.T.);
#8097=EDGE_CURVE('',#6483,#6485,#593,.T.);
#8098=EDGE_CURVE('',#6486,#6487,#3989,.T.);
#8099=EDGE_CURVE('',#6486,#6484,#594,.T.);
#8100=EDGE_CURVE('',#6485,#6487,#595,.T.);
#8101=EDGE_CURVE('',#6488,#6489,#3990,.T.);
#8102=EDGE_CURVE('',#6488,#6486,#596,.T.);
#8103=EDGE_CURVE('',#6487,#6489,#597,.T.);
#8104=EDGE_CURVE('',#6490,#6491,#3991,.T.);
#8105=EDGE_CURVE('',#6490,#6488,#598,.T.);
#8106=EDGE_CURVE('',#6489,#6491,#599,.T.);
#8107=EDGE_CURVE('',#6492,#6493,#3992,.T.);
#8108=EDGE_CURVE('',#6492,#6490,#600,.T.);
#8109=EDGE_CURVE('',#6491,#6493,#601,.T.);
#8110=EDGE_CURVE('',#6494,#6495,#3993,.T.);
#8111=EDGE_CURVE('',#6494,#6492,#602,.T.);
#8112=EDGE_CURVE('',#6493,#6495,#603,.T.);
#8113=EDGE_CURVE('',#6496,#6497,#3994,.T.);
#8114=EDGE_CURVE('',#6496,#6498,#604,.T.);
#8115=EDGE_CURVE('',#6497,#6498,#5514,.T.);
#8116=EDGE_CURVE('',#6499,#6500,#3995,.T.);
#8117=EDGE_CURVE('',#6499,#6496,#605,.T.);
#8118=EDGE_CURVE('',#6501,#6497,#5515,.T.);
#8119=EDGE_CURVE('',#6500,#6501,#606,.T.);
#8120=EDGE_CURVE('',#6502,#6503,#3996,.T.);
#8121=EDGE_CURVE('',#6502,#6499,#607,.T.);
#8122=EDGE_CURVE('',#6503,#6500,#608,.T.);
#8123=EDGE_CURVE('',#6504,#6505,#3997,.T.);
#8124=EDGE_CURVE('',#6504,#6502,#609,.T.);
#8125=EDGE_CURVE('',#6505,#6503,#610,.T.);
#8126=EDGE_CURVE('',#6506,#6507,#3998,.T.);
#8127=EDGE_CURVE('',#6506,#6504,#611,.T.);
#8128=EDGE_CURVE('',#6507,#6505,#612,.T.);
#8129=EDGE_CURVE('',#6508,#6509,#3999,.T.);
#8130=EDGE_CURVE('',#6508,#6506,#613,.T.);
#8131=EDGE_CURVE('',#6509,#6507,#614,.T.);
#8132=EDGE_CURVE('',#6510,#6511,#4000,.T.);
#8133=EDGE_CURVE('',#6510,#6508,#615,.T.);
#8134=EDGE_CURVE('',#6511,#6509,#616,.T.);
#8135=EDGE_CURVE('',#6512,#6513,#4001,.T.);
#8136=EDGE_CURVE('',#6512,#6510,#617,.T.);
#8137=EDGE_CURVE('',#6513,#6511,#618,.T.);
#8138=EDGE_CURVE('',#6514,#6515,#4002,.T.);
#8139=EDGE_CURVE('',#6514,#6512,#619,.T.);
#8140=EDGE_CURVE('',#6515,#6513,#620,.T.);
#8141=EDGE_CURVE('',#6516,#6517,#4003,.T.);
#8142=EDGE_CURVE('',#6516,#6514,#621,.T.);
#8143=EDGE_CURVE('',#6517,#6515,#622,.T.);
#8144=EDGE_CURVE('',#6518,#6519,#4004,.T.);
#8145=EDGE_CURVE('',#6518,#6516,#623,.T.);
#8146=EDGE_CURVE('',#6519,#6517,#624,.T.);
#8147=EDGE_CURVE('',#6520,#6521,#4005,.T.);
#8148=EDGE_CURVE('',#6520,#6518,#625,.T.);
#8149=EDGE_CURVE('',#6521,#6519,#626,.T.);
#8150=EDGE_CURVE('',#6522,#6523,#4006,.T.);
#8151=EDGE_CURVE('',#6522,#6520,#627,.T.);
#8152=EDGE_CURVE('',#6523,#6521,#628,.T.);
#8153=EDGE_CURVE('',#6524,#6525,#4007,.T.);
#8154=EDGE_CURVE('',#6524,#6522,#629,.T.);
#8155=EDGE_CURVE('',#6525,#6523,#630,.T.);
#8156=EDGE_CURVE('',#6526,#6527,#4008,.T.);
#8157=EDGE_CURVE('',#6526,#6524,#631,.T.);
#8158=EDGE_CURVE('',#6527,#6525,#632,.T.);
#8159=EDGE_CURVE('',#6528,#6529,#4009,.T.);
#8160=EDGE_CURVE('',#6528,#6526,#633,.T.);
#8161=EDGE_CURVE('',#6529,#6527,#634,.T.);
#8162=EDGE_CURVE('',#6530,#6531,#4010,.T.);
#8163=EDGE_CURVE('',#6530,#6528,#635,.T.);
#8164=EDGE_CURVE('',#6531,#6529,#636,.T.);
#8165=EDGE_CURVE('',#6532,#6533,#4011,.T.);
#8166=EDGE_CURVE('',#6532,#6530,#637,.T.);
#8167=EDGE_CURVE('',#6533,#6531,#638,.T.);
#8168=EDGE_CURVE('',#6534,#6535,#4012,.T.);
#8169=EDGE_CURVE('',#6534,#6532,#639,.T.);
#8170=EDGE_CURVE('',#6535,#6533,#640,.T.);
#8171=EDGE_CURVE('',#6536,#6537,#4013,.T.);
#8172=EDGE_CURVE('',#6536,#6534,#641,.T.);
#8173=EDGE_CURVE('',#6537,#6535,#642,.T.);
#8174=EDGE_CURVE('',#6538,#6539,#4014,.T.);
#8175=EDGE_CURVE('',#6538,#6536,#643,.T.);
#8176=EDGE_CURVE('',#6539,#6537,#644,.T.);
#8177=EDGE_CURVE('',#6540,#6541,#4015,.T.);
#8178=EDGE_CURVE('',#6540,#6538,#645,.T.);
#8179=EDGE_CURVE('',#6541,#6539,#646,.T.);
#8180=EDGE_CURVE('',#6542,#6543,#4016,.T.);
#8181=EDGE_CURVE('',#6542,#6540,#647,.T.);
#8182=EDGE_CURVE('',#6543,#6541,#648,.T.);
#8183=EDGE_CURVE('',#6544,#6545,#4017,.T.);
#8184=EDGE_CURVE('',#6544,#6542,#649,.T.);
#8185=EDGE_CURVE('',#6545,#6543,#650,.T.);
#8186=EDGE_CURVE('',#6546,#6547,#4018,.T.);
#8187=EDGE_CURVE('',#6546,#6544,#651,.T.);
#8188=EDGE_CURVE('',#6547,#6545,#652,.T.);
#8189=EDGE_CURVE('',#6548,#6549,#4019,.T.);
#8190=EDGE_CURVE('',#6548,#6546,#653,.T.);
#8191=EDGE_CURVE('',#6549,#6547,#654,.T.);
#8192=EDGE_CURVE('',#6550,#6551,#4020,.T.);
#8193=EDGE_CURVE('',#6550,#6548,#655,.T.);
#8194=EDGE_CURVE('',#6551,#6549,#656,.T.);
#8195=EDGE_CURVE('',#6552,#6553,#4021,.T.);
#8196=EDGE_CURVE('',#6552,#6550,#657,.T.);
#8197=EDGE_CURVE('',#6553,#6551,#658,.T.);
#8198=EDGE_CURVE('',#6554,#6555,#4022,.T.);
#8199=EDGE_CURVE('',#6554,#6552,#659,.T.);
#8200=EDGE_CURVE('',#6555,#6553,#660,.T.);
#8201=EDGE_CURVE('',#6556,#6557,#4023,.T.);
#8202=EDGE_CURVE('',#6556,#6554,#661,.T.);
#8203=EDGE_CURVE('',#6557,#6555,#662,.T.);
#8204=EDGE_CURVE('',#6558,#6559,#4024,.T.);
#8205=EDGE_CURVE('',#6558,#6556,#663,.T.);
#8206=EDGE_CURVE('',#6559,#6557,#664,.T.);
#8207=EDGE_CURVE('',#6560,#6561,#4025,.T.);
#8208=EDGE_CURVE('',#6560,#6558,#665,.T.);
#8209=EDGE_CURVE('',#6561,#6559,#666,.T.);
#8210=EDGE_CURVE('',#6562,#6563,#4026,.T.);
#8211=EDGE_CURVE('',#6562,#6560,#667,.T.);
#8212=EDGE_CURVE('',#6563,#6561,#668,.T.);
#8213=EDGE_CURVE('',#6564,#6565,#4027,.T.);
#8214=EDGE_CURVE('',#6564,#6562,#669,.T.);
#8215=EDGE_CURVE('',#6565,#6563,#670,.T.);
#8216=EDGE_CURVE('',#6566,#6567,#4028,.T.);
#8217=EDGE_CURVE('',#6566,#6564,#671,.T.);
#8218=EDGE_CURVE('',#6567,#6565,#672,.T.);
#8219=EDGE_CURVE('',#6568,#6569,#4029,.T.);
#8220=EDGE_CURVE('',#6568,#6566,#673,.T.);
#8221=EDGE_CURVE('',#6569,#6567,#674,.T.);
#8222=EDGE_CURVE('',#6570,#6571,#4030,.T.);
#8223=EDGE_CURVE('',#6570,#6568,#675,.T.);
#8224=EDGE_CURVE('',#6571,#6569,#676,.T.);
#8225=EDGE_CURVE('',#6572,#6573,#4031,.T.);
#8226=EDGE_CURVE('',#6572,#6570,#677,.T.);
#8227=EDGE_CURVE('',#6573,#6571,#678,.T.);
#8228=EDGE_CURVE('',#6574,#6575,#4032,.T.);
#8229=EDGE_CURVE('',#6574,#6572,#679,.T.);
#8230=EDGE_CURVE('',#6575,#6573,#680,.T.);
#8231=EDGE_CURVE('',#6576,#6577,#4033,.T.);
#8232=EDGE_CURVE('',#6576,#6574,#681,.T.);
#8233=EDGE_CURVE('',#6577,#6575,#682,.T.);
#8234=EDGE_CURVE('',#6578,#6579,#4034,.T.);
#8235=EDGE_CURVE('',#6578,#6576,#683,.T.);
#8236=EDGE_CURVE('',#6579,#6577,#684,.T.);
#8237=EDGE_CURVE('',#6580,#6581,#4035,.T.);
#8238=EDGE_CURVE('',#6580,#6578,#685,.T.);
#8239=EDGE_CURVE('',#6581,#6579,#686,.T.);
#8240=EDGE_CURVE('',#6582,#6583,#4036,.T.);
#8241=EDGE_CURVE('',#6582,#6580,#687,.T.);
#8242=EDGE_CURVE('',#6583,#6581,#688,.T.);
#8243=EDGE_CURVE('',#6584,#6585,#4037,.T.);
#8244=EDGE_CURVE('',#6584,#6582,#689,.T.);
#8245=EDGE_CURVE('',#6585,#6583,#690,.T.);
#8246=EDGE_CURVE('',#6586,#6587,#4038,.T.);
#8247=EDGE_CURVE('',#6586,#6584,#691,.T.);
#8248=EDGE_CURVE('',#6587,#6585,#692,.T.);
#8249=EDGE_CURVE('',#6588,#6589,#4039,.T.);
#8250=EDGE_CURVE('',#6588,#6586,#693,.T.);
#8251=EDGE_CURVE('',#6589,#6587,#694,.T.);
#8252=EDGE_CURVE('',#6590,#6591,#4040,.T.);
#8253=EDGE_CURVE('',#6590,#6588,#695,.T.);
#8254=EDGE_CURVE('',#6591,#6589,#696,.T.);
#8255=EDGE_CURVE('',#6592,#6593,#4041,.T.);
#8256=EDGE_CURVE('',#6592,#6590,#697,.T.);
#8257=EDGE_CURVE('',#6593,#6591,#698,.T.);
#8258=EDGE_CURVE('',#6594,#6595,#4042,.T.);
#8259=EDGE_CURVE('',#6594,#6592,#699,.T.);
#8260=EDGE_CURVE('',#6595,#6593,#700,.T.);
#8261=EDGE_CURVE('',#6596,#6597,#4043,.T.);
#8262=EDGE_CURVE('',#6596,#6594,#701,.T.);
#8263=EDGE_CURVE('',#6597,#6595,#702,.T.);
#8264=EDGE_CURVE('',#6598,#6599,#4044,.T.);
#8265=EDGE_CURVE('',#6598,#6596,#703,.T.);
#8266=EDGE_CURVE('',#6599,#6597,#704,.T.);
#8267=EDGE_CURVE('',#6600,#6601,#4045,.T.);
#8268=EDGE_CURVE('',#6600,#6598,#705,.T.);
#8269=EDGE_CURVE('',#6601,#6599,#706,.T.);
#8270=EDGE_CURVE('',#6602,#6603,#4046,.T.);
#8271=EDGE_CURVE('',#6602,#6600,#707,.T.);
#8272=EDGE_CURVE('',#6603,#6601,#708,.T.);
#8273=EDGE_CURVE('',#6604,#6605,#4047,.T.);
#8274=EDGE_CURVE('',#6604,#6602,#709,.T.);
#8275=EDGE_CURVE('',#6605,#6603,#710,.T.);
#8276=EDGE_CURVE('',#6606,#6607,#4048,.T.);
#8277=EDGE_CURVE('',#6606,#6604,#711,.T.);
#8278=EDGE_CURVE('',#6607,#6605,#712,.T.);
#8279=EDGE_CURVE('',#6608,#6609,#4049,.T.);
#8280=EDGE_CURVE('',#6608,#6606,#713,.T.);
#8281=EDGE_CURVE('',#6609,#6607,#714,.T.);
#8282=EDGE_CURVE('',#6610,#6611,#4050,.T.);
#8283=EDGE_CURVE('',#6610,#6608,#715,.T.);
#8284=EDGE_CURVE('',#6611,#6609,#716,.T.);
#8285=EDGE_CURVE('',#6612,#6613,#4051,.T.);
#8286=EDGE_CURVE('',#6612,#6610,#717,.T.);
#8287=EDGE_CURVE('',#6613,#6611,#718,.T.);
#8288=EDGE_CURVE('',#6614,#6615,#4052,.T.);
#8289=EDGE_CURVE('',#6614,#6612,#719,.T.);
#8290=EDGE_CURVE('',#6615,#6613,#720,.T.);
#8291=EDGE_CURVE('',#6616,#6617,#4053,.T.);
#8292=EDGE_CURVE('',#6616,#6614,#721,.T.);
#8293=EDGE_CURVE('',#6617,#6615,#722,.T.);
#8294=EDGE_CURVE('',#6618,#6619,#4054,.T.);
#8295=EDGE_CURVE('',#6618,#6616,#723,.T.);
#8296=EDGE_CURVE('',#6619,#6617,#724,.T.);
#8297=EDGE_CURVE('',#6620,#6621,#4055,.T.);
#8298=EDGE_CURVE('',#6620,#6618,#725,.T.);
#8299=EDGE_CURVE('',#6621,#6619,#726,.T.);
#8300=EDGE_CURVE('',#6622,#6623,#4056,.T.);
#8301=EDGE_CURVE('',#6622,#6620,#727,.T.);
#8302=EDGE_CURVE('',#6623,#6621,#728,.T.);
#8303=EDGE_CURVE('',#6624,#6624,#5516,.T.);
#8304=EDGE_CURVE('',#6625,#6371,#729,.T.);
#8305=EDGE_CURVE('',#6370,#6626,#730,.T.);
#8306=EDGE_CURVE('',#6626,#6625,#5517,.T.);
#8307=EDGE_CURVE('',#6624,#6627,#4057,.T.);
#8308=EDGE_CURVE('',#6627,#6627,#5518,.T.);
#8309=EDGE_CURVE('',#6628,#6501,#731,.T.);
#8310=EDGE_CURVE('',#6495,#6628,#732,.T.);
#8311=EDGE_CURVE('',#6625,#6623,#733,.T.);
#8312=EDGE_CURVE('',#6626,#6622,#734,.T.);
#8313=EDGE_CURVE('',#6498,#6629,#735,.T.);
#8314=EDGE_CURVE('',#6629,#6494,#736,.T.);
#8315=EDGE_CURVE('',#6630,#6631,#4058,.T.);
#8316=EDGE_CURVE('',#6630,#6632,#4059,.T.);
#8317=EDGE_CURVE('',#6633,#6632,#4060,.T.);
#8318=EDGE_CURVE('',#6631,#6633,#4061,.T.);
#8319=EDGE_CURVE('',#6631,#6634,#5519,.T.);
#8320=EDGE_CURVE('',#6633,#6635,#4062,.T.);
#8321=EDGE_CURVE('',#6635,#6634,#4063,.T.);
#8322=EDGE_CURVE('',#6632,#6636,#4064,.T.);
#8323=EDGE_CURVE('',#6635,#6636,#4065,.T.);
#8324=EDGE_CURVE('',#6634,#6637,#4066,.T.);
#8325=EDGE_CURVE('',#6636,#6637,#4067,.T.);
#8326=EDGE_CURVE('',#6637,#6630,#5520,.T.);
#8327=EDGE_CURVE('',#6638,#6638,#5521,.T.);
#8328=EDGE_CURVE('',#6638,#6639,#4068,.T.);
#8329=EDGE_CURVE('',#6639,#6639,#5522,.T.);
#8330=EDGE_CURVE('',#6640,#6640,#5523,.T.);
#8331=EDGE_CURVE('',#6629,#6628,#5524,.F.);
#8332=EDGE_CURVE('',#6641,#6641,#5525,.T.);
#8333=EDGE_CURVE('',#6641,#6640,#4069,.T.);
#8334=EDGE_CURVE('',#6642,#6642,#5526,.T.);
#8335=EDGE_CURVE('',#6642,#6643,#4070,.T.);
#8336=EDGE_CURVE('',#6643,#6643,#5527,.T.);
#8337=EDGE_CURVE('',#6644,#6644,#5528,.T.);
#8338=EDGE_CURVE('',#6644,#6645,#4071,.T.);
#8339=EDGE_CURVE('',#6645,#6645,#5529,.T.);
#8340=EDGE_CURVE('',#6646,#6647,#4072,.T.);
#8341=EDGE_CURVE('',#6646,#6647,#5530,.T.);
#8342=EDGE_CURVE('',#6648,#6649,#737,.T.);
#8343=EDGE_CURVE('',#6650,#6648,#5531,.T.);
#8344=EDGE_CURVE('',#6647,#6650,#738,.T.);
#8345=EDGE_CURVE('',#6649,#6646,#739,.T.);
#8346=EDGE_CURVE('',#6649,#6651,#4073,.T.);
#8347=EDGE_CURVE('',#6652,#6651,#740,.T.);
#8348=EDGE_CURVE('',#6651,#6652,#741,.T.);
#8349=EDGE_CURVE('',#6650,#6648,#4074,.T.);
#8350=EDGE_CURVE('',#6653,#6653,#5532,.T.);
#8351=EDGE_CURVE('',#6653,#6654,#4075,.T.);
#8352=EDGE_CURVE('',#6654,#6654,#5533,.T.);
#8353=EDGE_CURVE('',#6655,#6655,#5534,.T.);
#8354=EDGE_CURVE('',#6655,#6656,#4076,.T.);
#8355=EDGE_CURVE('',#6656,#6656,#5535,.T.);
#8356=EDGE_CURVE('',#6657,#6657,#5536,.T.);
#8357=EDGE_CURVE('',#6657,#6658,#4077,.T.);
#8358=EDGE_CURVE('',#6658,#6658,#5537,.T.);
#8359=EDGE_CURVE('',#6659,#6660,#4078,.T.);
#8360=EDGE_CURVE('',#6659,#6660,#5538,.T.);
#8361=EDGE_CURVE('',#6661,#6662,#742,.T.);
#8362=EDGE_CURVE('',#6663,#6661,#5539,.T.);
#8363=EDGE_CURVE('',#6660,#6663,#743,.T.);
#8364=EDGE_CURVE('',#6662,#6659,#744,.T.);
#8365=EDGE_CURVE('',#6662,#6664,#4079,.T.);
#8366=EDGE_CURVE('',#6665,#6664,#745,.T.);
#8367=EDGE_CURVE('',#6664,#6665,#746,.T.);
#8368=EDGE_CURVE('',#6663,#6661,#4080,.T.);
#8369=EDGE_CURVE('',#6666,#6667,#4081,.T.);
#8370=EDGE_CURVE('',#6668,#6666,#4082,.T.);
#8371=EDGE_CURVE('',#6669,#6668,#4083,.T.);
#8372=EDGE_CURVE('',#6670,#6669,#4084,.T.);
#8373=EDGE_CURVE('',#6671,#6670,#4085,.T.);
#8374=EDGE_CURVE('',#6667,#6671,#4086,.T.);
#8375=EDGE_CURVE('',#6672,#6666,#4087,.T.);
#8376=EDGE_CURVE('',#6673,#6672,#4088,.T.);
#8377=EDGE_CURVE('',#6668,#6673,#4089,.T.);
#8378=EDGE_CURVE('',#6674,#6672,#4090,.T.);
#8379=EDGE_CURVE('',#6675,#6674,#4091,.T.);
#8380=EDGE_CURVE('',#6676,#6675,#4092,.T.);
#8381=EDGE_CURVE('',#6677,#6676,#4093,.T.);
#8382=EDGE_CURVE('',#6673,#6677,#4094,.T.);
#8383=EDGE_CURVE('',#6678,#6678,#5540,.T.);
#8384=EDGE_CURVE('',#6667,#6674,#5541,.T.);
#8385=EDGE_CURVE('',#6679,#6679,#5542,.T.);
#8386=EDGE_CURVE('',#6677,#6669,#5543,.T.);
#8387=EDGE_CURVE('',#6678,#6679,#4095,.T.);
#8388=EDGE_CURVE('',#6671,#6675,#5544,.T.);
#8389=EDGE_CURVE('',#6676,#6670,#5545,.T.);
#8390=EDGE_CURVE('',#6680,#6680,#5546,.T.);
#8391=EDGE_CURVE('',#6680,#6681,#4096,.T.);
#8392=EDGE_CURVE('',#6681,#6681,#5547,.T.);
#8393=EDGE_CURVE('',#6682,#6682,#5548,.T.);
#8394=EDGE_CURVE('',#6682,#6683,#4097,.T.);
#8395=EDGE_CURVE('',#6683,#6683,#5549,.T.);
#8396=EDGE_CURVE('',#6684,#6684,#5550,.T.);
#8397=EDGE_CURVE('',#6684,#6685,#4098,.T.);
#8398=EDGE_CURVE('',#6685,#6685,#5551,.T.);
#8399=EDGE_CURVE('',#6686,#6686,#5552,.T.);
#8400=EDGE_CURVE('',#6686,#6687,#4099,.T.);
#8401=EDGE_CURVE('',#6687,#6687,#5553,.T.);
#8402=EDGE_CURVE('',#6688,#6689,#4100,.T.);
#8403=EDGE_CURVE('',#6690,#6688,#4101,.T.);
#8404=EDGE_CURVE('',#6691,#6690,#4102,.T.);
#8405=EDGE_CURVE('',#6692,#6691,#4103,.T.);
#8406=EDGE_CURVE('',#6693,#6692,#4104,.T.);
#8407=EDGE_CURVE('',#6694,#6693,#4105,.T.);
#8408=EDGE_CURVE('',#6695,#6694,#4106,.T.);
#8409=EDGE_CURVE('',#6689,#6695,#4107,.T.);
#8410=EDGE_CURVE('',#6692,#6696,#4108,.T.);
#8411=EDGE_CURVE('',#6696,#6697,#4109,.T.);
#8412=EDGE_CURVE('',#6697,#6693,#4110,.T.);
#8413=EDGE_CURVE('',#6698,#6691,#4111,.T.);
#8414=EDGE_CURVE('',#6698,#6696,#4112,.T.);
#8415=EDGE_CURVE('',#6690,#6699,#4113,.T.);
#8416=EDGE_CURVE('',#6699,#6698,#4114,.T.);
#8417=EDGE_CURVE('',#6700,#6688,#4115,.T.);
#8418=EDGE_CURVE('',#6700,#6699,#4116,.T.);
#8419=EDGE_CURVE('',#6701,#6702,#4117,.T.);
#8420=EDGE_CURVE('',#6697,#6701,#4118,.T.);
#8421=EDGE_CURVE('',#6703,#6700,#4119,.T.);
#8422=EDGE_CURVE('',#6702,#6703,#4120,.T.);
#8423=EDGE_CURVE('',#6694,#6701,#4121,.T.);
#8424=EDGE_CURVE('',#6689,#6703,#4122,.T.);
#8425=EDGE_CURVE('',#6702,#6695,#4123,.T.);
#8426=EDGE_CURVE('',#6704,#6705,#4124,.T.);
#8427=EDGE_CURVE('',#6704,#6706,#4125,.T.);
#8428=EDGE_CURVE('',#6706,#6707,#4126,.T.);
#8429=EDGE_CURVE('',#6705,#6707,#4127,.T.);
#8430=EDGE_CURVE('',#6708,#6704,#4128,.T.);
#8431=EDGE_CURVE('',#6708,#6709,#4129,.T.);
#8432=EDGE_CURVE('',#6709,#6706,#4130,.T.);
#8433=EDGE_CURVE('',#6710,#6708,#4131,.T.);
#8434=EDGE_CURVE('',#6710,#6711,#4132,.T.);
#8435=EDGE_CURVE('',#6711,#6709,#4133,.T.);
#8436=EDGE_CURVE('',#6712,#6710,#4134,.T.);
#8437=EDGE_CURVE('',#6712,#6713,#4135,.T.);
#8438=EDGE_CURVE('',#6713,#6711,#4136,.T.);
#8439=EDGE_CURVE('',#6714,#6712,#4137,.T.);
#8440=EDGE_CURVE('',#6714,#6715,#4138,.T.);
#8441=EDGE_CURVE('',#6715,#6713,#4139,.T.);
#8442=EDGE_CURVE('',#6705,#6714,#4140,.T.);
#8443=EDGE_CURVE('',#6707,#6715,#4141,.T.);
#8444=EDGE_CURVE('',#6716,#6716,#5554,.T.);
#8445=EDGE_CURVE('',#6717,#6717,#5555,.T.);
#8446=EDGE_CURVE('',#6717,#6716,#4142,.T.);
#8447=EDGE_CURVE('',#6718,#6718,#5556,.F.);
#8448=EDGE_CURVE('',#6718,#6717,#4143,.T.);
#8449=EDGE_CURVE('',#6719,#6719,#5557,.T.);
#8450=EDGE_CURVE('',#6719,#6718,#4144,.T.);
#8451=EDGE_CURVE('',#6720,#6720,#5558,.T.);
#8452=EDGE_CURVE('',#6720,#6721,#4145,.T.);
#8453=EDGE_CURVE('',#6721,#6721,#5559,.T.);
#8454=EDGE_CURVE('',#6722,#6722,#5560,.T.);
#8455=EDGE_CURVE('',#6722,#6723,#4146,.T.);
#8456=EDGE_CURVE('',#6723,#6723,#5561,.T.);
#8457=EDGE_CURVE('',#6724,#6724,#5562,.T.);
#8458=EDGE_CURVE('',#6725,#6725,#5563,.T.);
#8459=EDGE_CURVE('',#6725,#6724,#4147,.T.);
#8460=EDGE_CURVE('',#6726,#6726,#5564,.T.);
#8461=EDGE_CURVE('',#6726,#6725,#4148,.T.);
#8462=EDGE_CURVE('',#6727,#6727,#5565,.T.);
#8463=EDGE_CURVE('',#6727,#6726,#4149,.T.);
#8464=EDGE_CURVE('',#6728,#6728,#5566,.T.);
#8465=EDGE_CURVE('',#6729,#6729,#5567,.F.);
#8466=EDGE_CURVE('',#6729,#6728,#4150,.T.);
#8467=EDGE_CURVE('',#6730,#6730,#5568,.F.);
#8468=EDGE_CURVE('',#6730,#6729,#4151,.T.);
#8469=EDGE_CURVE('',#6731,#6731,#5569,.T.);
#8470=EDGE_CURVE('',#6731,#6730,#4152,.T.);
#8471=EDGE_CURVE('',#6732,#6733,#4153,.T.);
#8472=EDGE_CURVE('',#6733,#6734,#4154,.T.);
#8473=EDGE_CURVE('',#6734,#6735,#4155,.T.);
#8474=EDGE_CURVE('',#6732,#6735,#4156,.T.);
#8475=EDGE_CURVE('',#6733,#6736,#4157,.T.);
#8476=EDGE_CURVE('',#6736,#6737,#4158,.T.);
#8477=EDGE_CURVE('',#6737,#6734,#4159,.T.);
#8478=EDGE_CURVE('',#6736,#6738,#4160,.T.);
#8479=EDGE_CURVE('',#6738,#6739,#4161,.T.);
#8480=EDGE_CURVE('',#6739,#6737,#4162,.T.);
#8481=EDGE_CURVE('',#6738,#6740,#4163,.T.);
#8482=EDGE_CURVE('',#6740,#6741,#4164,.T.);
#8483=EDGE_CURVE('',#6741,#6739,#4165,.T.);
#8484=EDGE_CURVE('',#6740,#6742,#4166,.T.);
#8485=EDGE_CURVE('',#6742,#6743,#4167,.T.);
#8486=EDGE_CURVE('',#6743,#6741,#4168,.T.);
#8487=EDGE_CURVE('',#6742,#6732,#4169,.T.);
#8488=EDGE_CURVE('',#6735,#6743,#4170,.T.);
#8489=ORIENTED_EDGE('',*,*,#6744,.F.);
#8490=ORIENTED_EDGE('',*,*,#6745,.T.);
#8491=ORIENTED_EDGE('',*,*,#6746,.F.);
#8492=ORIENTED_EDGE('',*,*,#6745,.F.);
#8493=ORIENTED_EDGE('',*,*,#6747,.F.);
#8494=ORIENTED_EDGE('',*,*,#6748,.T.);
#8495=ORIENTED_EDGE('',*,*,#6749,.F.);
#8496=ORIENTED_EDGE('',*,*,#6748,.F.);
#8497=ORIENTED_EDGE('',*,*,#6750,.F.);
#8498=ORIENTED_EDGE('',*,*,#6751,.T.);
#8499=ORIENTED_EDGE('',*,*,#6752,.F.);
#8500=ORIENTED_EDGE('',*,*,#6751,.F.);
#8501=ORIENTED_EDGE('',*,*,#6753,.F.);
#8502=ORIENTED_EDGE('',*,*,#6754,.T.);
#8503=ORIENTED_EDGE('',*,*,#6755,.F.);
#8504=ORIENTED_EDGE('',*,*,#6754,.F.);
#8505=ORIENTED_EDGE('',*,*,#6756,.F.);
#8506=ORIENTED_EDGE('',*,*,#6757,.T.);
#8507=ORIENTED_EDGE('',*,*,#6758,.F.);
#8508=ORIENTED_EDGE('',*,*,#6757,.F.);
#8509=ORIENTED_EDGE('',*,*,#6759,.F.);
#8510=ORIENTED_EDGE('',*,*,#6760,.T.);
#8511=ORIENTED_EDGE('',*,*,#6761,.F.);
#8512=ORIENTED_EDGE('',*,*,#6760,.F.);
#8513=ORIENTED_EDGE('',*,*,#6762,.F.);
#8514=ORIENTED_EDGE('',*,*,#6763,.T.);
#8515=ORIENTED_EDGE('',*,*,#6764,.F.);
#8516=ORIENTED_EDGE('',*,*,#6763,.F.);
#8517=ORIENTED_EDGE('',*,*,#6765,.F.);
#8518=ORIENTED_EDGE('',*,*,#6766,.T.);
#8519=ORIENTED_EDGE('',*,*,#6767,.F.);
#8520=ORIENTED_EDGE('',*,*,#6766,.F.);
#8521=ORIENTED_EDGE('',*,*,#6768,.F.);
#8522=ORIENTED_EDGE('',*,*,#6769,.T.);
#8523=ORIENTED_EDGE('',*,*,#6770,.F.);
#8524=ORIENTED_EDGE('',*,*,#6769,.F.);
#8525=ORIENTED_EDGE('',*,*,#6771,.F.);
#8526=ORIENTED_EDGE('',*,*,#6772,.T.);
#8527=ORIENTED_EDGE('',*,*,#6773,.F.);
#8528=ORIENTED_EDGE('',*,*,#6772,.F.);
#8529=ORIENTED_EDGE('',*,*,#6774,.F.);
#8530=ORIENTED_EDGE('',*,*,#6775,.T.);
#8531=ORIENTED_EDGE('',*,*,#6776,.F.);
#8532=ORIENTED_EDGE('',*,*,#6775,.F.);
#8533=ORIENTED_EDGE('',*,*,#6777,.F.);
#8534=ORIENTED_EDGE('',*,*,#6778,.T.);
#8535=ORIENTED_EDGE('',*,*,#6779,.F.);
#8536=ORIENTED_EDGE('',*,*,#6778,.F.);
#8537=ORIENTED_EDGE('',*,*,#6780,.F.);
#8538=ORIENTED_EDGE('',*,*,#6781,.T.);
#8539=ORIENTED_EDGE('',*,*,#6782,.F.);
#8540=ORIENTED_EDGE('',*,*,#6781,.F.);
#8541=ORIENTED_EDGE('',*,*,#6783,.F.);
#8542=ORIENTED_EDGE('',*,*,#6784,.T.);
#8543=ORIENTED_EDGE('',*,*,#6785,.F.);
#8544=ORIENTED_EDGE('',*,*,#6784,.F.);
#8545=ORIENTED_EDGE('',*,*,#6786,.F.);
#8546=ORIENTED_EDGE('',*,*,#6787,.T.);
#8547=ORIENTED_EDGE('',*,*,#6788,.F.);
#8548=ORIENTED_EDGE('',*,*,#6787,.F.);
#8549=ORIENTED_EDGE('',*,*,#6789,.F.);
#8550=ORIENTED_EDGE('',*,*,#6790,.T.);
#8551=ORIENTED_EDGE('',*,*,#6791,.F.);
#8552=ORIENTED_EDGE('',*,*,#6790,.F.);
#8553=ORIENTED_EDGE('',*,*,#6792,.T.);
#8554=ORIENTED_EDGE('',*,*,#6793,.T.);
#8555=ORIENTED_EDGE('',*,*,#6794,.F.);
#8556=ORIENTED_EDGE('',*,*,#6795,.F.);
#8557=ORIENTED_EDGE('',*,*,#6796,.T.);
#8558=ORIENTED_EDGE('',*,*,#6795,.T.);
#8559=ORIENTED_EDGE('',*,*,#6797,.F.);
#8560=ORIENTED_EDGE('',*,*,#6798,.F.);
#8561=ORIENTED_EDGE('',*,*,#6799,.T.);
#8562=ORIENTED_EDGE('',*,*,#6798,.T.);
#8563=ORIENTED_EDGE('',*,*,#6800,.F.);
#8564=ORIENTED_EDGE('',*,*,#6801,.F.);
#8565=ORIENTED_EDGE('',*,*,#6802,.T.);
#8566=ORIENTED_EDGE('',*,*,#6801,.T.);
#8567=ORIENTED_EDGE('',*,*,#6803,.F.);
#8568=ORIENTED_EDGE('',*,*,#6793,.F.);
#8569=ORIENTED_EDGE('',*,*,#6803,.T.);
#8570=ORIENTED_EDGE('',*,*,#6800,.T.);
#8571=ORIENTED_EDGE('',*,*,#6797,.T.);
#8572=ORIENTED_EDGE('',*,*,#6794,.T.);
#8573=ORIENTED_EDGE('',*,*,#6758,.T.);
#8574=ORIENTED_EDGE('',*,*,#6761,.T.);
#8575=ORIENTED_EDGE('',*,*,#6770,.T.);
#8576=ORIENTED_EDGE('',*,*,#6773,.T.);
#8577=ORIENTED_EDGE('',*,*,#6776,.T.);
#8578=ORIENTED_EDGE('',*,*,#6779,.T.);
#8579=ORIENTED_EDGE('',*,*,#6782,.T.);
#8580=ORIENTED_EDGE('',*,*,#6785,.T.);
#8581=ORIENTED_EDGE('',*,*,#6788,.T.);
#8582=ORIENTED_EDGE('',*,*,#6791,.T.);
#8583=ORIENTED_EDGE('',*,*,#6767,.T.);
#8584=ORIENTED_EDGE('',*,*,#6764,.T.);
#8585=ORIENTED_EDGE('',*,*,#6755,.T.);
#8586=ORIENTED_EDGE('',*,*,#6752,.T.);
#8587=ORIENTED_EDGE('',*,*,#6749,.T.);
#8588=ORIENTED_EDGE('',*,*,#6746,.T.);
#8589=ORIENTED_EDGE('',*,*,#6802,.F.);
#8590=ORIENTED_EDGE('',*,*,#6792,.F.);
#8591=ORIENTED_EDGE('',*,*,#6796,.F.);
#8592=ORIENTED_EDGE('',*,*,#6799,.F.);
#8593=ORIENTED_EDGE('',*,*,#6756,.T.);
#8594=ORIENTED_EDGE('',*,*,#6759,.T.);
#8595=ORIENTED_EDGE('',*,*,#6768,.T.);
#8596=ORIENTED_EDGE('',*,*,#6771,.T.);
#8597=ORIENTED_EDGE('',*,*,#6774,.T.);
#8598=ORIENTED_EDGE('',*,*,#6777,.T.);
#8599=ORIENTED_EDGE('',*,*,#6780,.T.);
#8600=ORIENTED_EDGE('',*,*,#6783,.T.);
#8601=ORIENTED_EDGE('',*,*,#6786,.T.);
#8602=ORIENTED_EDGE('',*,*,#6789,.T.);
#8603=ORIENTED_EDGE('',*,*,#6765,.T.);
#8604=ORIENTED_EDGE('',*,*,#6762,.T.);
#8605=ORIENTED_EDGE('',*,*,#6753,.T.);
#8606=ORIENTED_EDGE('',*,*,#6750,.T.);
#8607=ORIENTED_EDGE('',*,*,#6747,.T.);
#8608=ORIENTED_EDGE('',*,*,#6744,.T.);
#8609=ORIENTED_EDGE('',*,*,#6804,.F.);
#8610=ORIENTED_EDGE('',*,*,#6805,.T.);
#8611=ORIENTED_EDGE('',*,*,#6806,.F.);
#8612=ORIENTED_EDGE('',*,*,#6805,.F.);
#8613=ORIENTED_EDGE('',*,*,#6807,.F.);
#8614=ORIENTED_EDGE('',*,*,#6808,.T.);
#8615=ORIENTED_EDGE('',*,*,#6809,.F.);
#8616=ORIENTED_EDGE('',*,*,#6808,.F.);
#8617=ORIENTED_EDGE('',*,*,#6810,.F.);
#8618=ORIENTED_EDGE('',*,*,#6811,.T.);
#8619=ORIENTED_EDGE('',*,*,#6812,.F.);
#8620=ORIENTED_EDGE('',*,*,#6811,.F.);
#8621=ORIENTED_EDGE('',*,*,#6813,.F.);
#8622=ORIENTED_EDGE('',*,*,#6814,.T.);
#8623=ORIENTED_EDGE('',*,*,#6815,.F.);
#8624=ORIENTED_EDGE('',*,*,#6814,.F.);
#8625=ORIENTED_EDGE('',*,*,#6816,.F.);
#8626=ORIENTED_EDGE('',*,*,#6817,.T.);
#8627=ORIENTED_EDGE('',*,*,#6818,.F.);
#8628=ORIENTED_EDGE('',*,*,#6817,.F.);
#8629=ORIENTED_EDGE('',*,*,#6816,.T.);
#8630=ORIENTED_EDGE('',*,*,#6819,.F.);
#8631=ORIENTED_EDGE('',*,*,#6820,.F.);
#8632=ORIENTED_EDGE('',*,*,#6821,.T.);
#8633=ORIENTED_EDGE('',*,*,#6822,.F.);
#8634=ORIENTED_EDGE('',*,*,#6821,.F.);
#8635=ORIENTED_EDGE('',*,*,#6820,.T.);
#8636=ORIENTED_EDGE('',*,*,#6823,.F.);
#8637=ORIENTED_EDGE('',*,*,#6824,.F.);
#8638=ORIENTED_EDGE('',*,*,#6825,.T.);
#8639=ORIENTED_EDGE('',*,*,#6826,.F.);
#8640=ORIENTED_EDGE('',*,*,#6825,.F.);
#8641=ORIENTED_EDGE('',*,*,#6824,.T.);
#8642=ORIENTED_EDGE('',*,*,#6827,.F.);
#8643=ORIENTED_EDGE('',*,*,#6828,.F.);
#8644=ORIENTED_EDGE('',*,*,#6829,.T.);
#8645=ORIENTED_EDGE('',*,*,#6830,.F.);
#8646=ORIENTED_EDGE('',*,*,#6829,.F.);
#8647=ORIENTED_EDGE('',*,*,#6828,.T.);
#8648=ORIENTED_EDGE('',*,*,#6831,.F.);
#8649=ORIENTED_EDGE('',*,*,#6832,.F.);
#8650=ORIENTED_EDGE('',*,*,#6833,.T.);
#8651=ORIENTED_EDGE('',*,*,#6819,.T.);
#8652=ORIENTED_EDGE('',*,*,#6833,.F.);
#8653=ORIENTED_EDGE('',*,*,#6834,.F.);
#8654=ORIENTED_EDGE('',*,*,#6835,.T.);
#8655=ORIENTED_EDGE('',*,*,#6823,.T.);
#8656=ORIENTED_EDGE('',*,*,#6835,.F.);
#8657=ORIENTED_EDGE('',*,*,#6836,.F.);
#8658=ORIENTED_EDGE('',*,*,#6837,.T.);
#8659=ORIENTED_EDGE('',*,*,#6827,.T.);
#8660=ORIENTED_EDGE('',*,*,#6837,.F.);
#8661=ORIENTED_EDGE('',*,*,#6838,.F.);
#8662=ORIENTED_EDGE('',*,*,#6839,.T.);
#8663=ORIENTED_EDGE('',*,*,#6831,.T.);
#8664=ORIENTED_EDGE('',*,*,#6839,.F.);
#8665=ORIENTED_EDGE('',*,*,#6840,.T.);
#8666=ORIENTED_EDGE('',*,*,#6841,.T.);
#8667=ORIENTED_EDGE('',*,*,#6842,.F.);
#8668=ORIENTED_EDGE('',*,*,#6843,.F.);
#8669=ORIENTED_EDGE('',*,*,#6844,.T.);
#8670=ORIENTED_EDGE('',*,*,#6843,.T.);
#8671=ORIENTED_EDGE('',*,*,#6845,.F.);
#8672=ORIENTED_EDGE('',*,*,#6846,.F.);
#8673=ORIENTED_EDGE('',*,*,#6847,.T.);
#8674=ORIENTED_EDGE('',*,*,#6846,.T.);
#8675=ORIENTED_EDGE('',*,*,#6848,.F.);
#8676=ORIENTED_EDGE('',*,*,#6849,.F.);
#8677=ORIENTED_EDGE('',*,*,#6850,.T.);
#8678=ORIENTED_EDGE('',*,*,#6849,.T.);
#8679=ORIENTED_EDGE('',*,*,#6851,.F.);
#8680=ORIENTED_EDGE('',*,*,#6841,.F.);
#8681=ORIENTED_EDGE('',*,*,#6851,.T.);
#8682=ORIENTED_EDGE('',*,*,#6848,.T.);
#8683=ORIENTED_EDGE('',*,*,#6845,.T.);
#8684=ORIENTED_EDGE('',*,*,#6842,.T.);
#8685=ORIENTED_EDGE('',*,*,#6818,.T.);
#8686=ORIENTED_EDGE('',*,*,#6822,.T.);
#8687=ORIENTED_EDGE('',*,*,#6826,.T.);
#8688=ORIENTED_EDGE('',*,*,#6830,.T.);
#8689=ORIENTED_EDGE('',*,*,#6815,.T.);
#8690=ORIENTED_EDGE('',*,*,#6812,.T.);
#8691=ORIENTED_EDGE('',*,*,#6809,.T.);
#8692=ORIENTED_EDGE('',*,*,#6806,.T.);
#8693=ORIENTED_EDGE('',*,*,#6850,.F.);
#8694=ORIENTED_EDGE('',*,*,#6840,.F.);
#8695=ORIENTED_EDGE('',*,*,#6844,.F.);
#8696=ORIENTED_EDGE('',*,*,#6847,.F.);
#8697=ORIENTED_EDGE('',*,*,#6838,.T.);
#8698=ORIENTED_EDGE('',*,*,#6836,.T.);
#8699=ORIENTED_EDGE('',*,*,#6834,.T.);
#8700=ORIENTED_EDGE('',*,*,#6832,.T.);
#8701=ORIENTED_EDGE('',*,*,#6813,.T.);
#8702=ORIENTED_EDGE('',*,*,#6810,.T.);
#8703=ORIENTED_EDGE('',*,*,#6807,.T.);
#8704=ORIENTED_EDGE('',*,*,#6804,.T.);
#8705=ORIENTED_EDGE('',*,*,#6852,.F.);
#8706=ORIENTED_EDGE('',*,*,#6853,.T.);
#8707=ORIENTED_EDGE('',*,*,#6854,.F.);
#8708=ORIENTED_EDGE('',*,*,#6853,.F.);
#8709=ORIENTED_EDGE('',*,*,#6855,.F.);
#8710=ORIENTED_EDGE('',*,*,#6856,.T.);
#8711=ORIENTED_EDGE('',*,*,#6857,.F.);
#8712=ORIENTED_EDGE('',*,*,#6856,.F.);
#8713=ORIENTED_EDGE('',*,*,#6858,.F.);
#8714=ORIENTED_EDGE('',*,*,#6859,.T.);
#8715=ORIENTED_EDGE('',*,*,#6860,.F.);
#8716=ORIENTED_EDGE('',*,*,#6859,.F.);
#8717=ORIENTED_EDGE('',*,*,#6861,.F.);
#8718=ORIENTED_EDGE('',*,*,#6862,.T.);
#8719=ORIENTED_EDGE('',*,*,#6863,.T.);
#8720=ORIENTED_EDGE('',*,*,#6862,.F.);
#8721=ORIENTED_EDGE('',*,*,#6863,.F.);
#8722=ORIENTED_EDGE('',*,*,#6864,.F.);
#8723=ORIENTED_EDGE('',*,*,#6864,.T.);
#8724=ORIENTED_EDGE('',*,*,#6865,.T.);
#8725=ORIENTED_EDGE('',*,*,#6866,.F.);
#8726=ORIENTED_EDGE('',*,*,#6865,.F.);
#8727=ORIENTED_EDGE('',*,*,#6867,.F.);
#8728=ORIENTED_EDGE('',*,*,#6868,.T.);
#8729=ORIENTED_EDGE('',*,*,#6869,.T.);
#8730=ORIENTED_EDGE('',*,*,#6868,.F.);
#8731=ORIENTED_EDGE('',*,*,#6869,.F.);
#8732=ORIENTED_EDGE('',*,*,#6870,.F.);
#8733=ORIENTED_EDGE('',*,*,#6871,.T.);
#8734=ORIENTED_EDGE('',*,*,#6872,.T.);
#8735=ORIENTED_EDGE('',*,*,#6871,.F.);
#8736=ORIENTED_EDGE('',*,*,#6872,.F.);
#8737=ORIENTED_EDGE('',*,*,#6873,.T.);
#8738=ORIENTED_EDGE('',*,*,#6874,.T.);
#8739=ORIENTED_EDGE('',*,*,#6875,.F.);
#8740=ORIENTED_EDGE('',*,*,#6876,.F.);
#8741=ORIENTED_EDGE('',*,*,#6877,.T.);
#8742=ORIENTED_EDGE('',*,*,#6876,.T.);
#8743=ORIENTED_EDGE('',*,*,#6878,.F.);
#8744=ORIENTED_EDGE('',*,*,#6879,.F.);
#8745=ORIENTED_EDGE('',*,*,#6854,.T.);
#8746=ORIENTED_EDGE('',*,*,#6857,.T.);
#8747=ORIENTED_EDGE('',*,*,#6860,.T.);
#8748=ORIENTED_EDGE('',*,*,#6866,.T.);
#8749=ORIENTED_EDGE('',*,*,#6880,.T.);
#8750=ORIENTED_EDGE('',*,*,#6879,.T.);
#8751=ORIENTED_EDGE('',*,*,#6881,.F.);
#8752=ORIENTED_EDGE('',*,*,#6882,.F.);
#8753=ORIENTED_EDGE('',*,*,#6883,.T.);
#8754=ORIENTED_EDGE('',*,*,#6882,.T.);
#8755=ORIENTED_EDGE('',*,*,#6884,.F.);
#8756=ORIENTED_EDGE('',*,*,#6874,.F.);
#8757=ORIENTED_EDGE('',*,*,#6852,.T.);
#8758=ORIENTED_EDGE('',*,*,#6855,.T.);
#8759=ORIENTED_EDGE('',*,*,#6858,.T.);
#8760=ORIENTED_EDGE('',*,*,#6861,.T.);
#8761=ORIENTED_EDGE('',*,*,#6884,.T.);
#8762=ORIENTED_EDGE('',*,*,#6881,.T.);
#8763=ORIENTED_EDGE('',*,*,#6878,.T.);
#8764=ORIENTED_EDGE('',*,*,#6875,.T.);
#8765=ORIENTED_EDGE('',*,*,#6883,.F.);
#8766=ORIENTED_EDGE('',*,*,#6873,.F.);
#8767=ORIENTED_EDGE('',*,*,#6877,.F.);
#8768=ORIENTED_EDGE('',*,*,#6880,.F.);
#8769=ORIENTED_EDGE('',*,*,#6867,.T.);
#8770=ORIENTED_EDGE('',*,*,#6870,.T.);
#8771=ORIENTED_EDGE('',*,*,#6885,.F.);
#8772=ORIENTED_EDGE('',*,*,#6886,.T.);
#8773=ORIENTED_EDGE('',*,*,#6887,.F.);
#8774=ORIENTED_EDGE('',*,*,#6886,.F.);
#8775=ORIENTED_EDGE('',*,*,#6888,.F.);
#8776=ORIENTED_EDGE('',*,*,#6889,.T.);
#8777=ORIENTED_EDGE('',*,*,#6890,.F.);
#8778=ORIENTED_EDGE('',*,*,#6889,.F.);
#8779=ORIENTED_EDGE('',*,*,#6891,.F.);
#8780=ORIENTED_EDGE('',*,*,#6892,.T.);
#8781=ORIENTED_EDGE('',*,*,#6893,.F.);
#8782=ORIENTED_EDGE('',*,*,#6892,.F.);
#8783=ORIENTED_EDGE('',*,*,#6894,.F.);
#8784=ORIENTED_EDGE('',*,*,#6895,.T.);
#8785=ORIENTED_EDGE('',*,*,#6896,.F.);
#8786=ORIENTED_EDGE('',*,*,#6895,.F.);
#8787=ORIENTED_EDGE('',*,*,#6894,.T.);
#8788=ORIENTED_EDGE('',*,*,#6897,.T.);
#8789=ORIENTED_EDGE('',*,*,#6897,.F.);
#8790=ORIENTED_EDGE('',*,*,#6898,.T.);
#8791=ORIENTED_EDGE('',*,*,#6899,.T.);
#8792=ORIENTED_EDGE('',*,*,#6898,.F.);
#8793=ORIENTED_EDGE('',*,*,#6900,.F.);
#8794=ORIENTED_EDGE('',*,*,#6901,.T.);
#8795=ORIENTED_EDGE('',*,*,#6902,.T.);
#8796=ORIENTED_EDGE('',*,*,#6901,.F.);
#8797=ORIENTED_EDGE('',*,*,#6900,.T.);
#8798=ORIENTED_EDGE('',*,*,#6887,.T.);
#8799=ORIENTED_EDGE('',*,*,#6890,.T.);
#8800=ORIENTED_EDGE('',*,*,#6893,.T.);
#8801=ORIENTED_EDGE('',*,*,#6896,.T.);
#8802=ORIENTED_EDGE('',*,*,#6902,.F.);
#8803=ORIENTED_EDGE('',*,*,#6885,.T.);
#8804=ORIENTED_EDGE('',*,*,#6888,.T.);
#8805=ORIENTED_EDGE('',*,*,#6891,.T.);
#8806=ORIENTED_EDGE('',*,*,#6899,.F.);
#8807=ORIENTED_EDGE('',*,*,#6903,.F.);
#8808=ORIENTED_EDGE('',*,*,#6904,.T.);
#8809=ORIENTED_EDGE('',*,*,#6905,.F.);
#8810=ORIENTED_EDGE('',*,*,#6904,.F.);
#8811=ORIENTED_EDGE('',*,*,#6906,.F.);
#8812=ORIENTED_EDGE('',*,*,#6907,.T.);
#8813=ORIENTED_EDGE('',*,*,#6908,.F.);
#8814=ORIENTED_EDGE('',*,*,#6907,.F.);
#8815=ORIENTED_EDGE('',*,*,#6909,.F.);
#8816=ORIENTED_EDGE('',*,*,#6910,.T.);
#8817=ORIENTED_EDGE('',*,*,#6911,.F.);
#8818=ORIENTED_EDGE('',*,*,#6910,.F.);
#8819=ORIENTED_EDGE('',*,*,#6912,.F.);
#8820=ORIENTED_EDGE('',*,*,#6913,.T.);
#8821=ORIENTED_EDGE('',*,*,#6914,.F.);
#8822=ORIENTED_EDGE('',*,*,#6913,.F.);
#8823=ORIENTED_EDGE('',*,*,#6912,.T.);
#8824=ORIENTED_EDGE('',*,*,#6915,.F.);
#8825=ORIENTED_EDGE('',*,*,#6916,.F.);
#8826=ORIENTED_EDGE('',*,*,#6917,.T.);
#8827=ORIENTED_EDGE('',*,*,#6915,.T.);
#8828=ORIENTED_EDGE('',*,*,#6917,.F.);
#8829=ORIENTED_EDGE('',*,*,#6918,.F.);
#8830=ORIENTED_EDGE('',*,*,#6919,.T.);
#8831=ORIENTED_EDGE('',*,*,#6920,.T.);
#8832=ORIENTED_EDGE('',*,*,#6919,.F.);
#8833=ORIENTED_EDGE('',*,*,#6920,.F.);
#8834=ORIENTED_EDGE('',*,*,#6921,.F.);
#8835=ORIENTED_EDGE('',*,*,#6922,.T.);
#8836=ORIENTED_EDGE('',*,*,#6923,.T.);
#8837=ORIENTED_EDGE('',*,*,#6922,.F.);
#8838=ORIENTED_EDGE('',*,*,#6923,.F.);
#8839=ORIENTED_EDGE('',*,*,#6924,.T.);
#8840=ORIENTED_EDGE('',*,*,#6925,.T.);
#8841=ORIENTED_EDGE('',*,*,#6926,.F.);
#8842=ORIENTED_EDGE('',*,*,#6927,.F.);
#8843=ORIENTED_EDGE('',*,*,#6928,.T.);
#8844=ORIENTED_EDGE('',*,*,#6927,.T.);
#8845=ORIENTED_EDGE('',*,*,#6929,.F.);
#8846=ORIENTED_EDGE('',*,*,#6930,.F.);
#8847=ORIENTED_EDGE('',*,*,#6905,.T.);
#8848=ORIENTED_EDGE('',*,*,#6908,.T.);
#8849=ORIENTED_EDGE('',*,*,#6911,.T.);
#8850=ORIENTED_EDGE('',*,*,#6914,.T.);
#8851=ORIENTED_EDGE('',*,*,#6931,.T.);
#8852=ORIENTED_EDGE('',*,*,#6930,.T.);
#8853=ORIENTED_EDGE('',*,*,#6932,.F.);
#8854=ORIENTED_EDGE('',*,*,#6933,.F.);
#8855=ORIENTED_EDGE('',*,*,#6934,.T.);
#8856=ORIENTED_EDGE('',*,*,#6933,.T.);
#8857=ORIENTED_EDGE('',*,*,#6935,.F.);
#8858=ORIENTED_EDGE('',*,*,#6925,.F.);
#8859=ORIENTED_EDGE('',*,*,#6903,.T.);
#8860=ORIENTED_EDGE('',*,*,#6906,.T.);
#8861=ORIENTED_EDGE('',*,*,#6909,.T.);
#8862=ORIENTED_EDGE('',*,*,#6916,.T.);
#8863=ORIENTED_EDGE('',*,*,#6935,.T.);
#8864=ORIENTED_EDGE('',*,*,#6932,.T.);
#8865=ORIENTED_EDGE('',*,*,#6929,.T.);
#8866=ORIENTED_EDGE('',*,*,#6926,.T.);
#8867=ORIENTED_EDGE('',*,*,#6934,.F.);
#8868=ORIENTED_EDGE('',*,*,#6924,.F.);
#8869=ORIENTED_EDGE('',*,*,#6928,.F.);
#8870=ORIENTED_EDGE('',*,*,#6931,.F.);
#8871=ORIENTED_EDGE('',*,*,#6918,.T.);
#8872=ORIENTED_EDGE('',*,*,#6921,.T.);
#8873=ORIENTED_EDGE('',*,*,#6936,.F.);
#8874=ORIENTED_EDGE('',*,*,#6937,.F.);
#8875=ORIENTED_EDGE('',*,*,#6938,.F.);
#8876=ORIENTED_EDGE('',*,*,#6939,.F.);
#8877=ORIENTED_EDGE('',*,*,#6937,.T.);
#8878=ORIENTED_EDGE('',*,*,#6940,.F.);
#8879=ORIENTED_EDGE('',*,*,#6941,.T.);
#8880=ORIENTED_EDGE('',*,*,#6942,.T.);
#8881=ORIENTED_EDGE('',*,*,#6943,.T.);
#8882=ORIENTED_EDGE('',*,*,#6944,.T.);
#8883=ORIENTED_EDGE('',*,*,#6938,.T.);
#8884=ORIENTED_EDGE('',*,*,#6940,.T.);
#8885=ORIENTED_EDGE('',*,*,#6936,.T.);
#8886=ORIENTED_EDGE('',*,*,#6945,.F.);
#8887=ORIENTED_EDGE('',*,*,#6944,.F.);
#8888=ORIENTED_EDGE('',*,*,#6946,.T.);
#8889=ORIENTED_EDGE('',*,*,#6947,.F.);
#8890=ORIENTED_EDGE('',*,*,#6946,.F.);
#8891=ORIENTED_EDGE('',*,*,#6943,.F.);
#8892=ORIENTED_EDGE('',*,*,#6948,.T.);
#8893=ORIENTED_EDGE('',*,*,#6949,.F.);
#8894=ORIENTED_EDGE('',*,*,#6948,.F.);
#8895=ORIENTED_EDGE('',*,*,#6942,.F.);
#8896=ORIENTED_EDGE('',*,*,#6950,.T.);
#8897=ORIENTED_EDGE('',*,*,#6951,.F.);
#8898=ORIENTED_EDGE('',*,*,#6950,.F.);
#8899=ORIENTED_EDGE('',*,*,#6941,.F.);
#8900=ORIENTED_EDGE('',*,*,#6952,.T.);
#8901=ORIENTED_EDGE('',*,*,#6953,.T.);
#8902=ORIENTED_EDGE('',*,*,#6952,.F.);
#8903=ORIENTED_EDGE('',*,*,#6953,.F.);
#8904=ORIENTED_EDGE('',*,*,#6954,.F.);
#8905=ORIENTED_EDGE('',*,*,#6955,.F.);
#8906=ORIENTED_EDGE('',*,*,#6956,.T.);
#8907=ORIENTED_EDGE('',*,*,#6954,.T.);
#8908=ORIENTED_EDGE('',*,*,#6956,.F.);
#8909=ORIENTED_EDGE('',*,*,#6939,.T.);
#8910=ORIENTED_EDGE('',*,*,#6945,.T.);
#8911=ORIENTED_EDGE('',*,*,#6947,.T.);
#8912=ORIENTED_EDGE('',*,*,#6949,.T.);
#8913=ORIENTED_EDGE('',*,*,#6951,.T.);
#8914=ORIENTED_EDGE('',*,*,#6955,.T.);
#8915=ORIENTED_EDGE('',*,*,#6957,.F.);
#8916=ORIENTED_EDGE('',*,*,#6958,.T.);
#8917=ORIENTED_EDGE('',*,*,#6959,.T.);
#8918=ORIENTED_EDGE('',*,*,#6960,.F.);
#8919=ORIENTED_EDGE('',*,*,#6961,.F.);
#8920=ORIENTED_EDGE('',*,*,#6962,.F.);
#8921=ORIENTED_EDGE('',*,*,#6963,.F.);
#8922=ORIENTED_EDGE('',*,*,#6959,.F.);
#8923=ORIENTED_EDGE('',*,*,#6964,.T.);
#8924=ORIENTED_EDGE('',*,*,#6965,.F.);
#8925=ORIENTED_EDGE('',*,*,#6964,.F.);
#8926=ORIENTED_EDGE('',*,*,#6958,.F.);
#8927=ORIENTED_EDGE('',*,*,#6966,.F.);
#8928=ORIENTED_EDGE('',*,*,#6967,.T.);
#8929=ORIENTED_EDGE('',*,*,#6968,.T.);
#8930=ORIENTED_EDGE('',*,*,#6969,.F.);
#8931=ORIENTED_EDGE('',*,*,#6970,.F.);
#8932=ORIENTED_EDGE('',*,*,#6971,.F.);
#8933=ORIENTED_EDGE('',*,*,#6972,.F.);
#8934=ORIENTED_EDGE('',*,*,#6968,.F.);
#8935=ORIENTED_EDGE('',*,*,#6973,.T.);
#8936=ORIENTED_EDGE('',*,*,#6974,.F.);
#8937=ORIENTED_EDGE('',*,*,#6973,.F.);
#8938=ORIENTED_EDGE('',*,*,#6967,.F.);
#8939=ORIENTED_EDGE('',*,*,#6961,.T.);
#8940=ORIENTED_EDGE('',*,*,#6957,.T.);
#8941=ORIENTED_EDGE('',*,*,#6963,.T.);
#8942=ORIENTED_EDGE('',*,*,#6975,.T.);
#8943=ORIENTED_EDGE('',*,*,#6976,.F.);
#8944=ORIENTED_EDGE('',*,*,#6977,.F.);
#8945=ORIENTED_EDGE('',*,*,#6978,.F.);
#8946=ORIENTED_EDGE('',*,*,#6979,.T.);
#8947=ORIENTED_EDGE('',*,*,#6970,.T.);
#8948=ORIENTED_EDGE('',*,*,#6966,.T.);
#8949=ORIENTED_EDGE('',*,*,#6972,.T.);
#8950=ORIENTED_EDGE('',*,*,#6980,.F.);
#8951=ORIENTED_EDGE('',*,*,#6981,.F.);
#8952=ORIENTED_EDGE('',*,*,#6982,.F.);
#8953=ORIENTED_EDGE('',*,*,#6983,.F.);
#8954=ORIENTED_EDGE('',*,*,#6984,.F.);
#8955=ORIENTED_EDGE('',*,*,#6985,.F.);
#8956=ORIENTED_EDGE('',*,*,#6986,.T.);
#8957=ORIENTED_EDGE('',*,*,#6960,.T.);
#8958=ORIENTED_EDGE('',*,*,#6986,.F.);
#8959=ORIENTED_EDGE('',*,*,#6987,.F.);
#8960=ORIENTED_EDGE('',*,*,#6988,.T.);
#8961=ORIENTED_EDGE('',*,*,#6969,.T.);
#8962=ORIENTED_EDGE('',*,*,#6988,.F.);
#8963=ORIENTED_EDGE('',*,*,#6962,.T.);
#8964=ORIENTED_EDGE('',*,*,#6979,.F.);
#8965=ORIENTED_EDGE('',*,*,#6989,.F.);
#8966=ORIENTED_EDGE('',*,*,#6980,.T.);
#8967=ORIENTED_EDGE('',*,*,#6971,.T.);
#8968=ORIENTED_EDGE('',*,*,#6984,.T.);
#8969=ORIENTED_EDGE('',*,*,#6990,.F.);
#8970=ORIENTED_EDGE('',*,*,#6975,.F.);
#8971=ORIENTED_EDGE('',*,*,#6976,.T.);
#8972=ORIENTED_EDGE('',*,*,#6990,.T.);
#8973=ORIENTED_EDGE('',*,*,#6983,.T.);
#8974=ORIENTED_EDGE('',*,*,#6991,.T.);
#8975=ORIENTED_EDGE('',*,*,#6992,.T.);
#8976=ORIENTED_EDGE('',*,*,#6993,.F.);
#8977=ORIENTED_EDGE('',*,*,#6994,.F.);
#8978=ORIENTED_EDGE('',*,*,#6995,.T.);
#8979=ORIENTED_EDGE('',*,*,#6982,.T.);
#8980=ORIENTED_EDGE('',*,*,#6996,.F.);
#8981=ORIENTED_EDGE('',*,*,#6997,.F.);
#8982=ORIENTED_EDGE('',*,*,#6991,.F.);
#8983=ORIENTED_EDGE('',*,*,#6987,.T.);
#8984=ORIENTED_EDGE('',*,*,#6997,.T.);
#8985=ORIENTED_EDGE('',*,*,#6998,.T.);
#8986=ORIENTED_EDGE('',*,*,#6999,.F.);
#8987=ORIENTED_EDGE('',*,*,#6992,.F.);
#8988=ORIENTED_EDGE('',*,*,#7000,.T.);
#8989=ORIENTED_EDGE('',*,*,#6994,.T.);
#8990=ORIENTED_EDGE('',*,*,#7001,.F.);
#8991=ORIENTED_EDGE('',*,*,#7002,.F.);
#8992=ORIENTED_EDGE('',*,*,#6978,.T.);
#8993=ORIENTED_EDGE('',*,*,#7003,.T.);
#8994=ORIENTED_EDGE('',*,*,#7002,.T.);
#8995=ORIENTED_EDGE('',*,*,#7004,.F.);
#8996=ORIENTED_EDGE('',*,*,#6998,.F.);
#8997=ORIENTED_EDGE('',*,*,#6996,.T.);
#8998=ORIENTED_EDGE('',*,*,#6981,.T.);
#8999=ORIENTED_EDGE('',*,*,#6989,.T.);
#9000=ORIENTED_EDGE('',*,*,#7004,.T.);
#9001=ORIENTED_EDGE('',*,*,#7001,.T.);
#9002=ORIENTED_EDGE('',*,*,#6993,.T.);
#9003=ORIENTED_EDGE('',*,*,#6999,.T.);
#9004=ORIENTED_EDGE('',*,*,#6965,.T.);
#9005=ORIENTED_EDGE('',*,*,#6974,.T.);
#9006=ORIENTED_EDGE('',*,*,#6977,.T.);
#9007=ORIENTED_EDGE('',*,*,#6995,.F.);
#9008=ORIENTED_EDGE('',*,*,#7000,.F.);
#9009=ORIENTED_EDGE('',*,*,#7003,.F.);
#9010=ORIENTED_EDGE('',*,*,#6985,.T.);
#9011=ORIENTED_EDGE('',*,*,#7005,.F.);
#9012=ORIENTED_EDGE('',*,*,#7006,.T.);
#9013=ORIENTED_EDGE('',*,*,#7007,.T.);
#9014=ORIENTED_EDGE('',*,*,#7008,.F.);
#9015=ORIENTED_EDGE('',*,*,#7009,.F.);
#9016=ORIENTED_EDGE('',*,*,#7010,.F.);
#9017=ORIENTED_EDGE('',*,*,#7011,.F.);
#9018=ORIENTED_EDGE('',*,*,#7007,.F.);
#9019=ORIENTED_EDGE('',*,*,#7012,.T.);
#9020=ORIENTED_EDGE('',*,*,#7013,.F.);
#9021=ORIENTED_EDGE('',*,*,#7012,.F.);
#9022=ORIENTED_EDGE('',*,*,#7006,.F.);
#9023=ORIENTED_EDGE('',*,*,#7014,.F.);
#9024=ORIENTED_EDGE('',*,*,#7015,.T.);
#9025=ORIENTED_EDGE('',*,*,#7016,.T.);
#9026=ORIENTED_EDGE('',*,*,#7017,.F.);
#9027=ORIENTED_EDGE('',*,*,#7018,.F.);
#9028=ORIENTED_EDGE('',*,*,#7019,.F.);
#9029=ORIENTED_EDGE('',*,*,#7020,.F.);
#9030=ORIENTED_EDGE('',*,*,#7016,.F.);
#9031=ORIENTED_EDGE('',*,*,#7021,.T.);
#9032=ORIENTED_EDGE('',*,*,#7022,.F.);
#9033=ORIENTED_EDGE('',*,*,#7021,.F.);
#9034=ORIENTED_EDGE('',*,*,#7015,.F.);
#9035=ORIENTED_EDGE('',*,*,#7009,.T.);
#9036=ORIENTED_EDGE('',*,*,#7005,.T.);
#9037=ORIENTED_EDGE('',*,*,#7011,.T.);
#9038=ORIENTED_EDGE('',*,*,#7023,.T.);
#9039=ORIENTED_EDGE('',*,*,#7024,.F.);
#9040=ORIENTED_EDGE('',*,*,#7025,.F.);
#9041=ORIENTED_EDGE('',*,*,#7026,.F.);
#9042=ORIENTED_EDGE('',*,*,#7027,.T.);
#9043=ORIENTED_EDGE('',*,*,#7018,.T.);
#9044=ORIENTED_EDGE('',*,*,#7014,.T.);
#9045=ORIENTED_EDGE('',*,*,#7020,.T.);
#9046=ORIENTED_EDGE('',*,*,#7028,.F.);
#9047=ORIENTED_EDGE('',*,*,#7029,.F.);
#9048=ORIENTED_EDGE('',*,*,#7030,.F.);
#9049=ORIENTED_EDGE('',*,*,#7031,.F.);
#9050=ORIENTED_EDGE('',*,*,#7032,.F.);
#9051=ORIENTED_EDGE('',*,*,#7033,.F.);
#9052=ORIENTED_EDGE('',*,*,#7034,.T.);
#9053=ORIENTED_EDGE('',*,*,#7008,.T.);
#9054=ORIENTED_EDGE('',*,*,#7034,.F.);
#9055=ORIENTED_EDGE('',*,*,#7035,.F.);
#9056=ORIENTED_EDGE('',*,*,#7036,.T.);
#9057=ORIENTED_EDGE('',*,*,#7017,.T.);
#9058=ORIENTED_EDGE('',*,*,#7036,.F.);
#9059=ORIENTED_EDGE('',*,*,#7010,.T.);
#9060=ORIENTED_EDGE('',*,*,#7027,.F.);
#9061=ORIENTED_EDGE('',*,*,#7037,.F.);
#9062=ORIENTED_EDGE('',*,*,#7028,.T.);
#9063=ORIENTED_EDGE('',*,*,#7019,.T.);
#9064=ORIENTED_EDGE('',*,*,#7032,.T.);
#9065=ORIENTED_EDGE('',*,*,#7038,.F.);
#9066=ORIENTED_EDGE('',*,*,#7023,.F.);
#9067=ORIENTED_EDGE('',*,*,#7024,.T.);
#9068=ORIENTED_EDGE('',*,*,#7038,.T.);
#9069=ORIENTED_EDGE('',*,*,#7031,.T.);
#9070=ORIENTED_EDGE('',*,*,#7039,.T.);
#9071=ORIENTED_EDGE('',*,*,#7040,.T.);
#9072=ORIENTED_EDGE('',*,*,#7041,.F.);
#9073=ORIENTED_EDGE('',*,*,#7042,.F.);
#9074=ORIENTED_EDGE('',*,*,#7043,.T.);
#9075=ORIENTED_EDGE('',*,*,#7030,.T.);
#9076=ORIENTED_EDGE('',*,*,#7044,.F.);
#9077=ORIENTED_EDGE('',*,*,#7045,.F.);
#9078=ORIENTED_EDGE('',*,*,#7039,.F.);
#9079=ORIENTED_EDGE('',*,*,#7035,.T.);
#9080=ORIENTED_EDGE('',*,*,#7045,.T.);
#9081=ORIENTED_EDGE('',*,*,#7046,.T.);
#9082=ORIENTED_EDGE('',*,*,#7047,.F.);
#9083=ORIENTED_EDGE('',*,*,#7040,.F.);
#9084=ORIENTED_EDGE('',*,*,#7048,.T.);
#9085=ORIENTED_EDGE('',*,*,#7042,.T.);
#9086=ORIENTED_EDGE('',*,*,#7049,.F.);
#9087=ORIENTED_EDGE('',*,*,#7050,.F.);
#9088=ORIENTED_EDGE('',*,*,#7026,.T.);
#9089=ORIENTED_EDGE('',*,*,#7051,.T.);
#9090=ORIENTED_EDGE('',*,*,#7050,.T.);
#9091=ORIENTED_EDGE('',*,*,#7052,.F.);
#9092=ORIENTED_EDGE('',*,*,#7046,.F.);
#9093=ORIENTED_EDGE('',*,*,#7044,.T.);
#9094=ORIENTED_EDGE('',*,*,#7029,.T.);
#9095=ORIENTED_EDGE('',*,*,#7037,.T.);
#9096=ORIENTED_EDGE('',*,*,#7052,.T.);
#9097=ORIENTED_EDGE('',*,*,#7049,.T.);
#9098=ORIENTED_EDGE('',*,*,#7041,.T.);
#9099=ORIENTED_EDGE('',*,*,#7047,.T.);
#9100=ORIENTED_EDGE('',*,*,#7013,.T.);
#9101=ORIENTED_EDGE('',*,*,#7022,.T.);
#9102=ORIENTED_EDGE('',*,*,#7025,.T.);
#9103=ORIENTED_EDGE('',*,*,#7043,.F.);
#9104=ORIENTED_EDGE('',*,*,#7048,.F.);
#9105=ORIENTED_EDGE('',*,*,#7051,.F.);
#9106=ORIENTED_EDGE('',*,*,#7033,.T.);
#9107=ORIENTED_EDGE('',*,*,#7053,.F.);
#9108=ORIENTED_EDGE('',*,*,#7054,.T.);
#9109=ORIENTED_EDGE('',*,*,#7055,.F.);
#9110=ORIENTED_EDGE('',*,*,#7054,.F.);
#9111=ORIENTED_EDGE('',*,*,#7053,.T.);
#9112=ORIENTED_EDGE('',*,*,#7056,.F.);
#9113=ORIENTED_EDGE('',*,*,#7057,.F.);
#9114=ORIENTED_EDGE('',*,*,#7058,.T.);
#9115=ORIENTED_EDGE('',*,*,#7059,.F.);
#9116=ORIENTED_EDGE('',*,*,#7058,.F.);
#9117=ORIENTED_EDGE('',*,*,#7057,.T.);
#9118=ORIENTED_EDGE('',*,*,#7060,.F.);
#9119=ORIENTED_EDGE('',*,*,#7061,.F.);
#9120=ORIENTED_EDGE('',*,*,#7062,.T.);
#9121=ORIENTED_EDGE('',*,*,#7063,.F.);
#9122=ORIENTED_EDGE('',*,*,#7062,.F.);
#9123=ORIENTED_EDGE('',*,*,#7061,.T.);
#9124=ORIENTED_EDGE('',*,*,#7064,.F.);
#9125=ORIENTED_EDGE('',*,*,#7065,.F.);
#9126=ORIENTED_EDGE('',*,*,#7066,.T.);
#9127=ORIENTED_EDGE('',*,*,#7067,.F.);
#9128=ORIENTED_EDGE('',*,*,#7066,.F.);
#9129=ORIENTED_EDGE('',*,*,#7065,.T.);
#9130=ORIENTED_EDGE('',*,*,#7068,.F.);
#9131=ORIENTED_EDGE('',*,*,#7069,.F.);
#9132=ORIENTED_EDGE('',*,*,#7070,.T.);
#9133=ORIENTED_EDGE('',*,*,#7056,.T.);
#9134=ORIENTED_EDGE('',*,*,#7070,.F.);
#9135=ORIENTED_EDGE('',*,*,#7071,.F.);
#9136=ORIENTED_EDGE('',*,*,#7072,.T.);
#9137=ORIENTED_EDGE('',*,*,#7060,.T.);
#9138=ORIENTED_EDGE('',*,*,#7072,.F.);
#9139=ORIENTED_EDGE('',*,*,#7073,.F.);
#9140=ORIENTED_EDGE('',*,*,#7074,.T.);
#9141=ORIENTED_EDGE('',*,*,#7064,.T.);
#9142=ORIENTED_EDGE('',*,*,#7074,.F.);
#9143=ORIENTED_EDGE('',*,*,#7075,.F.);
#9144=ORIENTED_EDGE('',*,*,#7076,.T.);
#9145=ORIENTED_EDGE('',*,*,#7068,.T.);
#9146=ORIENTED_EDGE('',*,*,#7076,.F.);
#9147=ORIENTED_EDGE('',*,*,#7077,.T.);
#9148=ORIENTED_EDGE('',*,*,#7078,.T.);
#9149=ORIENTED_EDGE('',*,*,#7079,.F.);
#9150=ORIENTED_EDGE('',*,*,#7080,.F.);
#9151=ORIENTED_EDGE('',*,*,#7081,.T.);
#9152=ORIENTED_EDGE('',*,*,#7080,.T.);
#9153=ORIENTED_EDGE('',*,*,#7082,.F.);
#9154=ORIENTED_EDGE('',*,*,#7083,.F.);
#9155=ORIENTED_EDGE('',*,*,#7084,.T.);
#9156=ORIENTED_EDGE('',*,*,#7083,.T.);
#9157=ORIENTED_EDGE('',*,*,#7085,.F.);
#9158=ORIENTED_EDGE('',*,*,#7086,.F.);
#9159=ORIENTED_EDGE('',*,*,#7087,.T.);
#9160=ORIENTED_EDGE('',*,*,#7086,.T.);
#9161=ORIENTED_EDGE('',*,*,#7088,.F.);
#9162=ORIENTED_EDGE('',*,*,#7089,.F.);
#9163=ORIENTED_EDGE('',*,*,#7090,.T.);
#9164=ORIENTED_EDGE('',*,*,#7089,.T.);
#9165=ORIENTED_EDGE('',*,*,#7091,.F.);
#9166=ORIENTED_EDGE('',*,*,#7092,.F.);
#9167=ORIENTED_EDGE('',*,*,#7067,.T.);
#9168=ORIENTED_EDGE('',*,*,#7063,.T.);
#9169=ORIENTED_EDGE('',*,*,#7059,.T.);
#9170=ORIENTED_EDGE('',*,*,#7055,.T.);
#9171=ORIENTED_EDGE('',*,*,#7093,.T.);
#9172=ORIENTED_EDGE('',*,*,#7092,.T.);
#9173=ORIENTED_EDGE('',*,*,#7094,.F.);
#9174=ORIENTED_EDGE('',*,*,#7095,.F.);
#9175=ORIENTED_EDGE('',*,*,#7096,.T.);
#9176=ORIENTED_EDGE('',*,*,#7095,.T.);
#9177=ORIENTED_EDGE('',*,*,#7097,.F.);
#9178=ORIENTED_EDGE('',*,*,#7098,.F.);
#9179=ORIENTED_EDGE('',*,*,#7099,.T.);
#9180=ORIENTED_EDGE('',*,*,#7098,.T.);
#9181=ORIENTED_EDGE('',*,*,#7100,.F.);
#9182=ORIENTED_EDGE('',*,*,#7101,.F.);
#9183=ORIENTED_EDGE('',*,*,#7102,.T.);
#9184=ORIENTED_EDGE('',*,*,#7101,.T.);
#9185=ORIENTED_EDGE('',*,*,#7103,.F.);
#9186=ORIENTED_EDGE('',*,*,#7104,.F.);
#9187=ORIENTED_EDGE('',*,*,#7105,.T.);
#9188=ORIENTED_EDGE('',*,*,#7104,.T.);
#9189=ORIENTED_EDGE('',*,*,#7106,.F.);
#9190=ORIENTED_EDGE('',*,*,#7107,.F.);
#9191=ORIENTED_EDGE('',*,*,#7108,.T.);
#9192=ORIENTED_EDGE('',*,*,#7107,.T.);
#9193=ORIENTED_EDGE('',*,*,#7109,.F.);
#9194=ORIENTED_EDGE('',*,*,#7110,.F.);
#9195=ORIENTED_EDGE('',*,*,#7069,.T.);
#9196=ORIENTED_EDGE('',*,*,#7071,.T.);
#9197=ORIENTED_EDGE('',*,*,#7073,.T.);
#9198=ORIENTED_EDGE('',*,*,#7075,.T.);
#9199=ORIENTED_EDGE('',*,*,#7111,.T.);
#9200=ORIENTED_EDGE('',*,*,#7110,.T.);
#9201=ORIENTED_EDGE('',*,*,#7112,.F.);
#9202=ORIENTED_EDGE('',*,*,#7078,.F.);
#9203=ORIENTED_EDGE('',*,*,#7112,.T.);
#9204=ORIENTED_EDGE('',*,*,#7109,.T.);
#9205=ORIENTED_EDGE('',*,*,#7106,.T.);
#9206=ORIENTED_EDGE('',*,*,#7103,.T.);
#9207=ORIENTED_EDGE('',*,*,#7100,.T.);
#9208=ORIENTED_EDGE('',*,*,#7097,.T.);
#9209=ORIENTED_EDGE('',*,*,#7094,.T.);
#9210=ORIENTED_EDGE('',*,*,#7091,.T.);
#9211=ORIENTED_EDGE('',*,*,#7088,.T.);
#9212=ORIENTED_EDGE('',*,*,#7085,.T.);
#9213=ORIENTED_EDGE('',*,*,#7082,.T.);
#9214=ORIENTED_EDGE('',*,*,#7079,.T.);
#9215=ORIENTED_EDGE('',*,*,#7111,.F.);
#9216=ORIENTED_EDGE('',*,*,#7077,.F.);
#9217=ORIENTED_EDGE('',*,*,#7081,.F.);
#9218=ORIENTED_EDGE('',*,*,#7084,.F.);
#9219=ORIENTED_EDGE('',*,*,#7087,.F.);
#9220=ORIENTED_EDGE('',*,*,#7090,.F.);
#9221=ORIENTED_EDGE('',*,*,#7093,.F.);
#9222=ORIENTED_EDGE('',*,*,#7096,.F.);
#9223=ORIENTED_EDGE('',*,*,#7099,.F.);
#9224=ORIENTED_EDGE('',*,*,#7102,.F.);
#9225=ORIENTED_EDGE('',*,*,#7105,.F.);
#9226=ORIENTED_EDGE('',*,*,#7108,.F.);
#9227=ORIENTED_EDGE('',*,*,#7113,.F.);
#9228=ORIENTED_EDGE('',*,*,#7114,.F.);
#9229=ORIENTED_EDGE('',*,*,#7115,.T.);
#9230=ORIENTED_EDGE('',*,*,#7116,.F.);
#9231=ORIENTED_EDGE('',*,*,#7117,.F.);
#9232=ORIENTED_EDGE('',*,*,#7115,.F.);
#9233=ORIENTED_EDGE('',*,*,#7116,.T.);
#9234=ORIENTED_EDGE('',*,*,#7117,.T.);
#9235=ORIENTED_EDGE('',*,*,#7118,.T.);
#9236=ORIENTED_EDGE('',*,*,#7119,.T.);
#9237=ORIENTED_EDGE('',*,*,#7118,.F.);
#9238=ORIENTED_EDGE('',*,*,#7120,.T.);
#9239=ORIENTED_EDGE('',*,*,#7121,.T.);
#9240=ORIENTED_EDGE('',*,*,#7122,.F.);
#9241=ORIENTED_EDGE('',*,*,#7121,.F.);
#9242=ORIENTED_EDGE('',*,*,#7122,.T.);
#9243=ORIENTED_EDGE('',*,*,#7123,.T.);
#9244=ORIENTED_EDGE('',*,*,#7124,.F.);
#9245=ORIENTED_EDGE('',*,*,#7123,.F.);
#9246=ORIENTED_EDGE('',*,*,#7119,.F.);
#9247=ORIENTED_EDGE('',*,*,#7124,.T.);
#9248=ORIENTED_EDGE('',*,*,#7125,.F.);
#9249=ORIENTED_EDGE('',*,*,#7126,.T.);
#9250=ORIENTED_EDGE('',*,*,#7113,.T.);
#9251=ORIENTED_EDGE('',*,*,#7114,.T.);
#9252=ORIENTED_EDGE('',*,*,#7126,.F.);
#9253=ORIENTED_EDGE('',*,*,#7125,.T.);
#9254=ORIENTED_EDGE('',*,*,#7127,.F.);
#9255=ORIENTED_EDGE('',*,*,#7127,.T.);
#9256=ORIENTED_EDGE('',*,*,#7128,.T.);
#9257=ORIENTED_EDGE('',*,*,#7120,.F.);
#9258=ORIENTED_EDGE('',*,*,#7128,.F.);
#9259=ORIENTED_EDGE('',*,*,#7129,.F.);
#9260=ORIENTED_EDGE('',*,*,#7130,.F.);
#9261=ORIENTED_EDGE('',*,*,#7131,.T.);
#9262=ORIENTED_EDGE('',*,*,#7132,.F.);
#9263=ORIENTED_EDGE('',*,*,#7133,.F.);
#9264=ORIENTED_EDGE('',*,*,#7131,.F.);
#9265=ORIENTED_EDGE('',*,*,#7134,.T.);
#9266=ORIENTED_EDGE('',*,*,#7135,.T.);
#9267=ORIENTED_EDGE('',*,*,#7132,.T.);
#9268=ORIENTED_EDGE('',*,*,#7133,.T.);
#9269=ORIENTED_EDGE('',*,*,#7135,.F.);
#9270=ORIENTED_EDGE('',*,*,#7136,.F.);
#9271=ORIENTED_EDGE('',*,*,#7137,.T.);
#9272=ORIENTED_EDGE('',*,*,#7138,.F.);
#9273=ORIENTED_EDGE('',*,*,#7139,.T.);
#9274=ORIENTED_EDGE('',*,*,#7136,.T.);
#9275=ORIENTED_EDGE('',*,*,#7139,.F.);
#9276=ORIENTED_EDGE('',*,*,#7140,.F.);
#9277=ORIENTED_EDGE('',*,*,#7141,.T.);
#9278=ORIENTED_EDGE('',*,*,#7138,.T.);
#9279=ORIENTED_EDGE('',*,*,#7141,.F.);
#9280=ORIENTED_EDGE('',*,*,#7142,.F.);
#9281=ORIENTED_EDGE('',*,*,#7143,.T.);
#9282=ORIENTED_EDGE('',*,*,#7140,.T.);
#9283=ORIENTED_EDGE('',*,*,#7143,.F.);
#9284=ORIENTED_EDGE('',*,*,#7142,.T.);
#9285=ORIENTED_EDGE('',*,*,#7134,.F.);
#9286=ORIENTED_EDGE('',*,*,#7129,.T.);
#9287=ORIENTED_EDGE('',*,*,#7130,.T.);
#9288=ORIENTED_EDGE('',*,*,#7144,.T.);
#9289=ORIENTED_EDGE('',*,*,#7137,.F.);
#9290=ORIENTED_EDGE('',*,*,#7144,.F.);
#9291=ORIENTED_EDGE('',*,*,#7145,.T.);
#9292=ORIENTED_EDGE('',*,*,#7145,.F.);
#9293=ORIENTED_EDGE('',*,*,#7146,.T.);
#9294=ORIENTED_EDGE('',*,*,#7146,.F.);
#9295=ORIENTED_EDGE('',*,*,#7147,.T.);
#9296=ORIENTED_EDGE('',*,*,#7147,.F.);
#9297=ORIENTED_EDGE('',*,*,#7148,.T.);
#9298=ORIENTED_EDGE('',*,*,#7148,.F.);
#9299=ORIENTED_EDGE('',*,*,#7149,.T.);
#9300=ORIENTED_EDGE('',*,*,#7149,.F.);
#9301=ORIENTED_EDGE('',*,*,#7150,.T.);
#9302=ORIENTED_EDGE('',*,*,#7150,.F.);
#9303=ORIENTED_EDGE('',*,*,#7151,.T.);
#9304=ORIENTED_EDGE('',*,*,#7151,.F.);
#9305=ORIENTED_EDGE('',*,*,#7152,.F.);
#9306=ORIENTED_EDGE('',*,*,#7153,.F.);
#9307=ORIENTED_EDGE('',*,*,#7154,.F.);
#9308=ORIENTED_EDGE('',*,*,#7155,.F.);
#9309=ORIENTED_EDGE('',*,*,#7154,.T.);
#9310=ORIENTED_EDGE('',*,*,#7156,.F.);
#9311=ORIENTED_EDGE('',*,*,#7157,.T.);
#9312=ORIENTED_EDGE('',*,*,#7158,.F.);
#9313=ORIENTED_EDGE('',*,*,#7159,.T.);
#9314=ORIENTED_EDGE('',*,*,#7160,.F.);
#9315=ORIENTED_EDGE('',*,*,#7161,.T.);
#9316=ORIENTED_EDGE('',*,*,#7162,.F.);
#9317=ORIENTED_EDGE('',*,*,#7161,.F.);
#9318=ORIENTED_EDGE('',*,*,#7163,.F.);
#9319=ORIENTED_EDGE('',*,*,#7164,.T.);
#9320=ORIENTED_EDGE('',*,*,#7165,.F.);
#9321=ORIENTED_EDGE('',*,*,#7166,.T.);
#9322=ORIENTED_EDGE('',*,*,#7167,.F.);
#9323=ORIENTED_EDGE('',*,*,#7168,.T.);
#9324=ORIENTED_EDGE('',*,*,#7169,.F.);
#9325=ORIENTED_EDGE('',*,*,#7170,.T.);
#9326=ORIENTED_EDGE('',*,*,#7171,.F.);
#9327=ORIENTED_EDGE('',*,*,#7153,.T.);
#9328=ORIENTED_EDGE('',*,*,#7172,.T.);
#9329=ORIENTED_EDGE('',*,*,#7173,.T.);
#9330=ORIENTED_EDGE('',*,*,#7156,.T.);
#9331=ORIENTED_EDGE('',*,*,#7174,.F.);
#9332=ORIENTED_EDGE('',*,*,#7175,.F.);
#9333=ORIENTED_EDGE('',*,*,#7157,.F.);
#9334=ORIENTED_EDGE('',*,*,#7173,.F.);
#9335=ORIENTED_EDGE('',*,*,#7175,.T.);
#9336=ORIENTED_EDGE('',*,*,#7176,.T.);
#9337=ORIENTED_EDGE('',*,*,#7177,.T.);
#9338=ORIENTED_EDGE('',*,*,#7158,.T.);
#9339=ORIENTED_EDGE('',*,*,#7178,.F.);
#9340=ORIENTED_EDGE('',*,*,#7179,.F.);
#9341=ORIENTED_EDGE('',*,*,#7159,.F.);
#9342=ORIENTED_EDGE('',*,*,#7177,.F.);
#9343=ORIENTED_EDGE('',*,*,#7179,.T.);
#9344=ORIENTED_EDGE('',*,*,#7180,.T.);
#9345=ORIENTED_EDGE('',*,*,#7181,.T.);
#9346=ORIENTED_EDGE('',*,*,#7182,.T.);
#9347=ORIENTED_EDGE('',*,*,#7163,.T.);
#9348=ORIENTED_EDGE('',*,*,#7160,.T.);
#9349=ORIENTED_EDGE('',*,*,#7183,.F.);
#9350=ORIENTED_EDGE('',*,*,#7184,.F.);
#9351=ORIENTED_EDGE('',*,*,#7164,.F.);
#9352=ORIENTED_EDGE('',*,*,#7182,.F.);
#9353=ORIENTED_EDGE('',*,*,#7184,.T.);
#9354=ORIENTED_EDGE('',*,*,#7185,.T.);
#9355=ORIENTED_EDGE('',*,*,#7186,.T.);
#9356=ORIENTED_EDGE('',*,*,#7165,.T.);
#9357=ORIENTED_EDGE('',*,*,#7187,.F.);
#9358=ORIENTED_EDGE('',*,*,#7188,.F.);
#9359=ORIENTED_EDGE('',*,*,#7166,.F.);
#9360=ORIENTED_EDGE('',*,*,#7186,.F.);
#9361=ORIENTED_EDGE('',*,*,#7188,.T.);
#9362=ORIENTED_EDGE('',*,*,#7189,.T.);
#9363=ORIENTED_EDGE('',*,*,#7190,.T.);
#9364=ORIENTED_EDGE('',*,*,#7167,.T.);
#9365=ORIENTED_EDGE('',*,*,#7168,.F.);
#9366=ORIENTED_EDGE('',*,*,#7190,.F.);
#9367=ORIENTED_EDGE('',*,*,#7191,.F.);
#9368=ORIENTED_EDGE('',*,*,#7192,.F.);
#9369=ORIENTED_EDGE('',*,*,#7193,.F.);
#9370=ORIENTED_EDGE('',*,*,#7194,.T.);
#9371=ORIENTED_EDGE('',*,*,#7180,.F.);
#9372=ORIENTED_EDGE('',*,*,#7178,.T.);
#9373=ORIENTED_EDGE('',*,*,#7176,.F.);
#9374=ORIENTED_EDGE('',*,*,#7174,.T.);
#9375=ORIENTED_EDGE('',*,*,#7172,.F.);
#9376=ORIENTED_EDGE('',*,*,#7152,.T.);
#9377=ORIENTED_EDGE('',*,*,#7195,.F.);
#9378=ORIENTED_EDGE('',*,*,#7196,.T.);
#9379=ORIENTED_EDGE('',*,*,#7197,.F.);
#9380=ORIENTED_EDGE('',*,*,#7191,.T.);
#9381=ORIENTED_EDGE('',*,*,#7189,.F.);
#9382=ORIENTED_EDGE('',*,*,#7187,.T.);
#9383=ORIENTED_EDGE('',*,*,#7185,.F.);
#9384=ORIENTED_EDGE('',*,*,#7183,.T.);
#9385=ORIENTED_EDGE('',*,*,#7181,.F.);
#9386=ORIENTED_EDGE('',*,*,#7194,.F.);
#9387=ORIENTED_EDGE('',*,*,#7155,.T.);
#9388=ORIENTED_EDGE('',*,*,#7171,.T.);
#9389=ORIENTED_EDGE('',*,*,#7198,.T.);
#9390=ORIENTED_EDGE('',*,*,#7195,.T.);
#9391=ORIENTED_EDGE('',*,*,#7170,.F.);
#9392=ORIENTED_EDGE('',*,*,#7199,.F.);
#9393=ORIENTED_EDGE('',*,*,#7196,.F.);
#9394=ORIENTED_EDGE('',*,*,#7198,.F.);
#9395=ORIENTED_EDGE('',*,*,#7162,.T.);
#9396=ORIENTED_EDGE('',*,*,#7193,.T.);
#9397=ORIENTED_EDGE('',*,*,#7192,.T.);
#9398=ORIENTED_EDGE('',*,*,#7197,.T.);
#9399=ORIENTED_EDGE('',*,*,#7199,.T.);
#9400=ORIENTED_EDGE('',*,*,#7169,.T.);
#9401=ORIENTED_EDGE('',*,*,#7200,.F.);
#9402=ORIENTED_EDGE('',*,*,#7201,.T.);
#9403=ORIENTED_EDGE('',*,*,#7202,.F.);
#9404=ORIENTED_EDGE('',*,*,#7203,.T.);
#9405=ORIENTED_EDGE('',*,*,#7200,.T.);
#9406=ORIENTED_EDGE('',*,*,#7203,.F.);
#9407=ORIENTED_EDGE('',*,*,#7202,.T.);
#9408=ORIENTED_EDGE('',*,*,#7204,.F.);
#9409=ORIENTED_EDGE('',*,*,#7204,.T.);
#9410=ORIENTED_EDGE('',*,*,#7205,.T.);
#9411=ORIENTED_EDGE('',*,*,#7201,.F.);
#9412=ORIENTED_EDGE('',*,*,#7205,.F.);
#9413=ORIENTED_EDGE('',*,*,#7206,.F.);
#9414=ORIENTED_EDGE('',*,*,#7207,.T.);
#9415=ORIENTED_EDGE('',*,*,#7208,.F.);
#9416=ORIENTED_EDGE('',*,*,#7209,.T.);
#9417=ORIENTED_EDGE('',*,*,#7206,.T.);
#9418=ORIENTED_EDGE('',*,*,#7209,.F.);
#9419=ORIENTED_EDGE('',*,*,#7208,.T.);
#9420=ORIENTED_EDGE('',*,*,#7210,.F.);
#9421=ORIENTED_EDGE('',*,*,#7210,.T.);
#9422=ORIENTED_EDGE('',*,*,#7211,.T.);
#9423=ORIENTED_EDGE('',*,*,#7207,.F.);
#9424=ORIENTED_EDGE('',*,*,#7211,.F.);
#9425=ORIENTED_EDGE('',*,*,#7212,.F.);
#9426=ORIENTED_EDGE('',*,*,#7213,.F.);
#9427=ORIENTED_EDGE('',*,*,#7214,.T.);
#9428=ORIENTED_EDGE('',*,*,#7215,.F.);
#9429=ORIENTED_EDGE('',*,*,#7216,.F.);
#9430=ORIENTED_EDGE('',*,*,#7214,.F.);
#9431=ORIENTED_EDGE('',*,*,#7215,.T.);
#9432=ORIENTED_EDGE('',*,*,#7216,.T.);
#9433=ORIENTED_EDGE('',*,*,#7217,.T.);
#9434=ORIENTED_EDGE('',*,*,#7218,.T.);
#9435=ORIENTED_EDGE('',*,*,#7217,.F.);
#9436=ORIENTED_EDGE('',*,*,#7219,.T.);
#9437=ORIENTED_EDGE('',*,*,#7220,.T.);
#9438=ORIENTED_EDGE('',*,*,#7221,.F.);
#9439=ORIENTED_EDGE('',*,*,#7220,.F.);
#9440=ORIENTED_EDGE('',*,*,#7221,.T.);
#9441=ORIENTED_EDGE('',*,*,#7222,.T.);
#9442=ORIENTED_EDGE('',*,*,#7223,.F.);
#9443=ORIENTED_EDGE('',*,*,#7222,.F.);
#9444=ORIENTED_EDGE('',*,*,#7218,.F.);
#9445=ORIENTED_EDGE('',*,*,#7223,.T.);
#9446=ORIENTED_EDGE('',*,*,#7224,.F.);
#9447=ORIENTED_EDGE('',*,*,#7225,.T.);
#9448=ORIENTED_EDGE('',*,*,#7212,.T.);
#9449=ORIENTED_EDGE('',*,*,#7213,.T.);
#9450=ORIENTED_EDGE('',*,*,#7225,.F.);
#9451=ORIENTED_EDGE('',*,*,#7224,.T.);
#9452=ORIENTED_EDGE('',*,*,#7226,.F.);
#9453=ORIENTED_EDGE('',*,*,#7226,.T.);
#9454=ORIENTED_EDGE('',*,*,#7227,.T.);
#9455=ORIENTED_EDGE('',*,*,#7219,.F.);
#9456=ORIENTED_EDGE('',*,*,#7227,.F.);
#9457=ORIENTED_EDGE('',*,*,#7228,.F.);
#9458=ORIENTED_EDGE('',*,*,#7229,.F.);
#9459=ORIENTED_EDGE('',*,*,#7230,.T.);
#9460=ORIENTED_EDGE('',*,*,#7231,.F.);
#9461=ORIENTED_EDGE('',*,*,#7232,.F.);
#9462=ORIENTED_EDGE('',*,*,#7230,.F.);
#9463=ORIENTED_EDGE('',*,*,#7233,.T.);
#9464=ORIENTED_EDGE('',*,*,#7234,.T.);
#9465=ORIENTED_EDGE('',*,*,#7231,.T.);
#9466=ORIENTED_EDGE('',*,*,#7232,.T.);
#9467=ORIENTED_EDGE('',*,*,#7234,.F.);
#9468=ORIENTED_EDGE('',*,*,#7235,.F.);
#9469=ORIENTED_EDGE('',*,*,#7236,.T.);
#9470=ORIENTED_EDGE('',*,*,#7237,.F.);
#9471=ORIENTED_EDGE('',*,*,#7238,.T.);
#9472=ORIENTED_EDGE('',*,*,#7235,.T.);
#9473=ORIENTED_EDGE('',*,*,#7238,.F.);
#9474=ORIENTED_EDGE('',*,*,#7239,.F.);
#9475=ORIENTED_EDGE('',*,*,#7240,.T.);
#9476=ORIENTED_EDGE('',*,*,#7237,.T.);
#9477=ORIENTED_EDGE('',*,*,#7240,.F.);
#9478=ORIENTED_EDGE('',*,*,#7241,.F.);
#9479=ORIENTED_EDGE('',*,*,#7242,.T.);
#9480=ORIENTED_EDGE('',*,*,#7239,.T.);
#9481=ORIENTED_EDGE('',*,*,#7242,.F.);
#9482=ORIENTED_EDGE('',*,*,#7241,.T.);
#9483=ORIENTED_EDGE('',*,*,#7233,.F.);
#9484=ORIENTED_EDGE('',*,*,#7228,.T.);
#9485=ORIENTED_EDGE('',*,*,#7229,.T.);
#9486=ORIENTED_EDGE('',*,*,#7243,.T.);
#9487=ORIENTED_EDGE('',*,*,#7236,.F.);
#9488=ORIENTED_EDGE('',*,*,#7243,.F.);
#9489=ORIENTED_EDGE('',*,*,#7244,.T.);
#9490=ORIENTED_EDGE('',*,*,#7244,.F.);
#9491=ORIENTED_EDGE('',*,*,#7245,.T.);
#9492=ORIENTED_EDGE('',*,*,#7245,.F.);
#9493=ORIENTED_EDGE('',*,*,#7246,.T.);
#9494=ORIENTED_EDGE('',*,*,#7246,.F.);
#9495=ORIENTED_EDGE('',*,*,#7247,.T.);
#9496=ORIENTED_EDGE('',*,*,#7247,.F.);
#9497=ORIENTED_EDGE('',*,*,#7248,.T.);
#9498=ORIENTED_EDGE('',*,*,#7248,.F.);
#9499=ORIENTED_EDGE('',*,*,#7249,.T.);
#9500=ORIENTED_EDGE('',*,*,#7249,.F.);
#9501=ORIENTED_EDGE('',*,*,#7250,.T.);
#9502=ORIENTED_EDGE('',*,*,#7250,.F.);
#9503=ORIENTED_EDGE('',*,*,#7251,.T.);
#9504=ORIENTED_EDGE('',*,*,#7251,.F.);
#9505=ORIENTED_EDGE('',*,*,#7252,.F.);
#9506=ORIENTED_EDGE('',*,*,#7253,.F.);
#9507=ORIENTED_EDGE('',*,*,#7254,.F.);
#9508=ORIENTED_EDGE('',*,*,#7255,.F.);
#9509=ORIENTED_EDGE('',*,*,#7254,.T.);
#9510=ORIENTED_EDGE('',*,*,#7256,.F.);
#9511=ORIENTED_EDGE('',*,*,#7257,.T.);
#9512=ORIENTED_EDGE('',*,*,#7258,.F.);
#9513=ORIENTED_EDGE('',*,*,#7259,.T.);
#9514=ORIENTED_EDGE('',*,*,#7260,.F.);
#9515=ORIENTED_EDGE('',*,*,#7261,.T.);
#9516=ORIENTED_EDGE('',*,*,#7262,.T.);
#9517=ORIENTED_EDGE('',*,*,#7263,.F.);
#9518=ORIENTED_EDGE('',*,*,#7262,.F.);
#9519=ORIENTED_EDGE('',*,*,#7264,.T.);
#9520=ORIENTED_EDGE('',*,*,#7265,.F.);
#9521=ORIENTED_EDGE('',*,*,#7266,.T.);
#9522=ORIENTED_EDGE('',*,*,#7267,.F.);
#9523=ORIENTED_EDGE('',*,*,#7268,.T.);
#9524=ORIENTED_EDGE('',*,*,#7269,.F.);
#9525=ORIENTED_EDGE('',*,*,#7270,.T.);
#9526=ORIENTED_EDGE('',*,*,#7271,.F.);
#9527=ORIENTED_EDGE('',*,*,#7272,.T.);
#9528=ORIENTED_EDGE('',*,*,#7273,.F.);
#9529=ORIENTED_EDGE('',*,*,#7253,.T.);
#9530=ORIENTED_EDGE('',*,*,#7274,.T.);
#9531=ORIENTED_EDGE('',*,*,#7275,.T.);
#9532=ORIENTED_EDGE('',*,*,#7256,.T.);
#9533=ORIENTED_EDGE('',*,*,#7276,.F.);
#9534=ORIENTED_EDGE('',*,*,#7277,.F.);
#9535=ORIENTED_EDGE('',*,*,#7257,.F.);
#9536=ORIENTED_EDGE('',*,*,#7275,.F.);
#9537=ORIENTED_EDGE('',*,*,#7277,.T.);
#9538=ORIENTED_EDGE('',*,*,#7278,.T.);
#9539=ORIENTED_EDGE('',*,*,#7279,.T.);
#9540=ORIENTED_EDGE('',*,*,#7258,.T.);
#9541=ORIENTED_EDGE('',*,*,#7280,.F.);
#9542=ORIENTED_EDGE('',*,*,#7281,.F.);
#9543=ORIENTED_EDGE('',*,*,#7259,.F.);
#9544=ORIENTED_EDGE('',*,*,#7279,.F.);
#9545=ORIENTED_EDGE('',*,*,#7281,.T.);
#9546=ORIENTED_EDGE('',*,*,#7282,.T.);
#9547=ORIENTED_EDGE('',*,*,#7283,.T.);
#9548=ORIENTED_EDGE('',*,*,#7260,.T.);
#9549=ORIENTED_EDGE('',*,*,#7284,.F.);
#9550=ORIENTED_EDGE('',*,*,#7285,.F.);
#9551=ORIENTED_EDGE('',*,*,#7264,.F.);
#9552=ORIENTED_EDGE('',*,*,#7261,.F.);
#9553=ORIENTED_EDGE('',*,*,#7283,.F.);
#9554=ORIENTED_EDGE('',*,*,#7286,.F.);
#9555=ORIENTED_EDGE('',*,*,#7285,.T.);
#9556=ORIENTED_EDGE('',*,*,#7287,.T.);
#9557=ORIENTED_EDGE('',*,*,#7288,.T.);
#9558=ORIENTED_EDGE('',*,*,#7265,.T.);
#9559=ORIENTED_EDGE('',*,*,#7289,.F.);
#9560=ORIENTED_EDGE('',*,*,#7290,.F.);
#9561=ORIENTED_EDGE('',*,*,#7266,.F.);
#9562=ORIENTED_EDGE('',*,*,#7288,.F.);
#9563=ORIENTED_EDGE('',*,*,#7290,.T.);
#9564=ORIENTED_EDGE('',*,*,#7291,.T.);
#9565=ORIENTED_EDGE('',*,*,#7292,.T.);
#9566=ORIENTED_EDGE('',*,*,#7267,.T.);
#9567=ORIENTED_EDGE('',*,*,#7293,.F.);
#9568=ORIENTED_EDGE('',*,*,#7294,.F.);
#9569=ORIENTED_EDGE('',*,*,#7268,.F.);
#9570=ORIENTED_EDGE('',*,*,#7292,.F.);
#9571=ORIENTED_EDGE('',*,*,#7294,.T.);
#9572=ORIENTED_EDGE('',*,*,#7295,.T.);
#9573=ORIENTED_EDGE('',*,*,#7296,.T.);
#9574=ORIENTED_EDGE('',*,*,#7269,.T.);
#9575=ORIENTED_EDGE('',*,*,#7270,.F.);
#9576=ORIENTED_EDGE('',*,*,#7296,.F.);
#9577=ORIENTED_EDGE('',*,*,#7297,.F.);
#9578=ORIENTED_EDGE('',*,*,#7298,.F.);
#9579=ORIENTED_EDGE('',*,*,#7299,.F.);
#9580=ORIENTED_EDGE('',*,*,#7300,.T.);
#9581=ORIENTED_EDGE('',*,*,#7286,.T.);
#9582=ORIENTED_EDGE('',*,*,#7282,.F.);
#9583=ORIENTED_EDGE('',*,*,#7280,.T.);
#9584=ORIENTED_EDGE('',*,*,#7278,.F.);
#9585=ORIENTED_EDGE('',*,*,#7276,.T.);
#9586=ORIENTED_EDGE('',*,*,#7274,.F.);
#9587=ORIENTED_EDGE('',*,*,#7252,.T.);
#9588=ORIENTED_EDGE('',*,*,#7301,.F.);
#9589=ORIENTED_EDGE('',*,*,#7302,.T.);
#9590=ORIENTED_EDGE('',*,*,#7303,.F.);
#9591=ORIENTED_EDGE('',*,*,#7297,.T.);
#9592=ORIENTED_EDGE('',*,*,#7295,.F.);
#9593=ORIENTED_EDGE('',*,*,#7293,.T.);
#9594=ORIENTED_EDGE('',*,*,#7291,.F.);
#9595=ORIENTED_EDGE('',*,*,#7289,.T.);
#9596=ORIENTED_EDGE('',*,*,#7287,.F.);
#9597=ORIENTED_EDGE('',*,*,#7284,.T.);
#9598=ORIENTED_EDGE('',*,*,#7300,.F.);
#9599=ORIENTED_EDGE('',*,*,#7255,.T.);
#9600=ORIENTED_EDGE('',*,*,#7273,.T.);
#9601=ORIENTED_EDGE('',*,*,#7304,.T.);
#9602=ORIENTED_EDGE('',*,*,#7301,.T.);
#9603=ORIENTED_EDGE('',*,*,#7272,.F.);
#9604=ORIENTED_EDGE('',*,*,#7305,.F.);
#9605=ORIENTED_EDGE('',*,*,#7302,.F.);
#9606=ORIENTED_EDGE('',*,*,#7304,.F.);
#9607=ORIENTED_EDGE('',*,*,#7263,.T.);
#9608=ORIENTED_EDGE('',*,*,#7299,.T.);
#9609=ORIENTED_EDGE('',*,*,#7298,.T.);
#9610=ORIENTED_EDGE('',*,*,#7303,.T.);
#9611=ORIENTED_EDGE('',*,*,#7305,.T.);
#9612=ORIENTED_EDGE('',*,*,#7271,.T.);
#9613=ORIENTED_EDGE('',*,*,#7306,.F.);
#9614=ORIENTED_EDGE('',*,*,#7307,.T.);
#9615=ORIENTED_EDGE('',*,*,#7308,.F.);
#9616=ORIENTED_EDGE('',*,*,#7309,.T.);
#9617=ORIENTED_EDGE('',*,*,#7306,.T.);
#9618=ORIENTED_EDGE('',*,*,#7309,.F.);
#9619=ORIENTED_EDGE('',*,*,#7308,.T.);
#9620=ORIENTED_EDGE('',*,*,#7310,.F.);
#9621=ORIENTED_EDGE('',*,*,#7310,.T.);
#9622=ORIENTED_EDGE('',*,*,#7311,.T.);
#9623=ORIENTED_EDGE('',*,*,#7307,.F.);
#9624=ORIENTED_EDGE('',*,*,#7311,.F.);
#9625=ORIENTED_EDGE('',*,*,#7312,.F.);
#9626=ORIENTED_EDGE('',*,*,#7313,.T.);
#9627=ORIENTED_EDGE('',*,*,#7314,.F.);
#9628=ORIENTED_EDGE('',*,*,#7315,.T.);
#9629=ORIENTED_EDGE('',*,*,#7312,.T.);
#9630=ORIENTED_EDGE('',*,*,#7315,.F.);
#9631=ORIENTED_EDGE('',*,*,#7314,.T.);
#9632=ORIENTED_EDGE('',*,*,#7316,.F.);
#9633=ORIENTED_EDGE('',*,*,#7316,.T.);
#9634=ORIENTED_EDGE('',*,*,#7317,.T.);
#9635=ORIENTED_EDGE('',*,*,#7313,.F.);
#9636=ORIENTED_EDGE('',*,*,#7317,.F.);
#9637=ORIENTED_EDGE('',*,*,#7318,.F.);
#9638=ORIENTED_EDGE('',*,*,#7319,.T.);
#9639=ORIENTED_EDGE('',*,*,#7320,.F.);
#9640=ORIENTED_EDGE('',*,*,#7321,.F.);
#9641=ORIENTED_EDGE('',*,*,#7322,.F.);
#9642=ORIENTED_EDGE('',*,*,#7323,.T.);
#9643=ORIENTED_EDGE('',*,*,#7324,.F.);
#9644=ORIENTED_EDGE('',*,*,#7319,.F.);
#9645=ORIENTED_EDGE('',*,*,#7325,.F.);
#9646=ORIENTED_EDGE('',*,*,#7326,.T.);
#9647=ORIENTED_EDGE('',*,*,#7327,.F.);
#9648=ORIENTED_EDGE('',*,*,#7323,.F.);
#9649=ORIENTED_EDGE('',*,*,#7328,.F.);
#9650=ORIENTED_EDGE('',*,*,#7329,.T.);
#9651=ORIENTED_EDGE('',*,*,#7330,.F.);
#9652=ORIENTED_EDGE('',*,*,#7326,.F.);
#9653=ORIENTED_EDGE('',*,*,#7331,.F.);
#9654=ORIENTED_EDGE('',*,*,#7332,.T.);
#9655=ORIENTED_EDGE('',*,*,#7333,.F.);
#9656=ORIENTED_EDGE('',*,*,#7329,.F.);
#9657=ORIENTED_EDGE('',*,*,#7334,.F.);
#9658=ORIENTED_EDGE('',*,*,#7335,.T.);
#9659=ORIENTED_EDGE('',*,*,#7336,.F.);
#9660=ORIENTED_EDGE('',*,*,#7332,.F.);
#9661=ORIENTED_EDGE('',*,*,#7337,.F.);
#9662=ORIENTED_EDGE('',*,*,#7338,.T.);
#9663=ORIENTED_EDGE('',*,*,#7339,.F.);
#9664=ORIENTED_EDGE('',*,*,#7335,.F.);
#9665=ORIENTED_EDGE('',*,*,#7340,.F.);
#9666=ORIENTED_EDGE('',*,*,#7341,.T.);
#9667=ORIENTED_EDGE('',*,*,#7342,.F.);
#9668=ORIENTED_EDGE('',*,*,#7338,.F.);
#9669=ORIENTED_EDGE('',*,*,#7343,.F.);
#9670=ORIENTED_EDGE('',*,*,#7344,.F.);
#9671=ORIENTED_EDGE('',*,*,#7345,.F.);
#9672=ORIENTED_EDGE('',*,*,#7341,.F.);
#9673=ORIENTED_EDGE('',*,*,#7346,.F.);
#9674=ORIENTED_EDGE('',*,*,#7347,.T.);
#9675=ORIENTED_EDGE('',*,*,#7348,.F.);
#9676=ORIENTED_EDGE('',*,*,#7349,.F.);
#9677=ORIENTED_EDGE('',*,*,#7350,.F.);
#9678=ORIENTED_EDGE('',*,*,#7351,.T.);
#9679=ORIENTED_EDGE('',*,*,#7352,.F.);
#9680=ORIENTED_EDGE('',*,*,#7347,.F.);
#9681=ORIENTED_EDGE('',*,*,#7353,.F.);
#9682=ORIENTED_EDGE('',*,*,#7354,.T.);
#9683=ORIENTED_EDGE('',*,*,#7355,.F.);
#9684=ORIENTED_EDGE('',*,*,#7351,.F.);
#9685=ORIENTED_EDGE('',*,*,#7356,.F.);
#9686=ORIENTED_EDGE('',*,*,#7357,.T.);
#9687=ORIENTED_EDGE('',*,*,#7358,.F.);
#9688=ORIENTED_EDGE('',*,*,#7354,.F.);
#9689=ORIENTED_EDGE('',*,*,#7359,.F.);
#9690=ORIENTED_EDGE('',*,*,#7360,.T.);
#9691=ORIENTED_EDGE('',*,*,#7361,.F.);
#9692=ORIENTED_EDGE('',*,*,#7357,.F.);
#9693=ORIENTED_EDGE('',*,*,#7362,.F.);
#9694=ORIENTED_EDGE('',*,*,#7363,.T.);
#9695=ORIENTED_EDGE('',*,*,#7364,.F.);
#9696=ORIENTED_EDGE('',*,*,#7360,.F.);
#9697=ORIENTED_EDGE('',*,*,#7365,.F.);
#9698=ORIENTED_EDGE('',*,*,#7366,.T.);
#9699=ORIENTED_EDGE('',*,*,#7367,.F.);
#9700=ORIENTED_EDGE('',*,*,#7363,.F.);
#9701=ORIENTED_EDGE('',*,*,#7368,.F.);
#9702=ORIENTED_EDGE('',*,*,#7369,.T.);
#9703=ORIENTED_EDGE('',*,*,#7370,.F.);
#9704=ORIENTED_EDGE('',*,*,#7366,.F.);
#9705=ORIENTED_EDGE('',*,*,#7371,.F.);
#9706=ORIENTED_EDGE('',*,*,#7372,.F.);
#9707=ORIENTED_EDGE('',*,*,#7373,.F.);
#9708=ORIENTED_EDGE('',*,*,#7369,.F.);
#9709=ORIENTED_EDGE('',*,*,#7374,.F.);
#9710=ORIENTED_EDGE('',*,*,#7375,.T.);
#9711=ORIENTED_EDGE('',*,*,#7376,.F.);
#9712=ORIENTED_EDGE('',*,*,#7377,.F.);
#9713=ORIENTED_EDGE('',*,*,#7378,.F.);
#9714=ORIENTED_EDGE('',*,*,#7379,.T.);
#9715=ORIENTED_EDGE('',*,*,#7380,.F.);
#9716=ORIENTED_EDGE('',*,*,#7375,.F.);
#9717=ORIENTED_EDGE('',*,*,#7381,.F.);
#9718=ORIENTED_EDGE('',*,*,#7382,.T.);
#9719=ORIENTED_EDGE('',*,*,#7383,.F.);
#9720=ORIENTED_EDGE('',*,*,#7379,.F.);
#9721=ORIENTED_EDGE('',*,*,#7384,.F.);
#9722=ORIENTED_EDGE('',*,*,#7385,.T.);
#9723=ORIENTED_EDGE('',*,*,#7386,.F.);
#9724=ORIENTED_EDGE('',*,*,#7382,.F.);
#9725=ORIENTED_EDGE('',*,*,#7387,.F.);
#9726=ORIENTED_EDGE('',*,*,#7388,.T.);
#9727=ORIENTED_EDGE('',*,*,#7389,.F.);
#9728=ORIENTED_EDGE('',*,*,#7385,.F.);
#9729=ORIENTED_EDGE('',*,*,#7390,.F.);
#9730=ORIENTED_EDGE('',*,*,#7391,.T.);
#9731=ORIENTED_EDGE('',*,*,#7392,.F.);
#9732=ORIENTED_EDGE('',*,*,#7388,.F.);
#9733=ORIENTED_EDGE('',*,*,#7393,.F.);
#9734=ORIENTED_EDGE('',*,*,#7394,.T.);
#9735=ORIENTED_EDGE('',*,*,#7395,.F.);
#9736=ORIENTED_EDGE('',*,*,#7391,.F.);
#9737=ORIENTED_EDGE('',*,*,#7396,.F.);
#9738=ORIENTED_EDGE('',*,*,#7397,.T.);
#9739=ORIENTED_EDGE('',*,*,#7398,.F.);
#9740=ORIENTED_EDGE('',*,*,#7394,.F.);
#9741=ORIENTED_EDGE('',*,*,#7399,.F.);
#9742=ORIENTED_EDGE('',*,*,#7400,.F.);
#9743=ORIENTED_EDGE('',*,*,#7401,.F.);
#9744=ORIENTED_EDGE('',*,*,#7397,.F.);
#9745=ORIENTED_EDGE('',*,*,#7402,.F.);
#9746=ORIENTED_EDGE('',*,*,#7403,.T.);
#9747=ORIENTED_EDGE('',*,*,#7404,.F.);
#9748=ORIENTED_EDGE('',*,*,#7405,.F.);
#9749=ORIENTED_EDGE('',*,*,#7406,.F.);
#9750=ORIENTED_EDGE('',*,*,#7407,.T.);
#9751=ORIENTED_EDGE('',*,*,#7408,.F.);
#9752=ORIENTED_EDGE('',*,*,#7403,.F.);
#9753=ORIENTED_EDGE('',*,*,#7409,.F.);
#9754=ORIENTED_EDGE('',*,*,#7410,.T.);
#9755=ORIENTED_EDGE('',*,*,#7411,.F.);
#9756=ORIENTED_EDGE('',*,*,#7407,.F.);
#9757=ORIENTED_EDGE('',*,*,#7412,.F.);
#9758=ORIENTED_EDGE('',*,*,#7413,.T.);
#9759=ORIENTED_EDGE('',*,*,#7414,.F.);
#9760=ORIENTED_EDGE('',*,*,#7410,.F.);
#9761=ORIENTED_EDGE('',*,*,#7415,.F.);
#9762=ORIENTED_EDGE('',*,*,#7416,.T.);
#9763=ORIENTED_EDGE('',*,*,#7417,.F.);
#9764=ORIENTED_EDGE('',*,*,#7413,.F.);
#9765=ORIENTED_EDGE('',*,*,#7418,.F.);
#9766=ORIENTED_EDGE('',*,*,#7419,.T.);
#9767=ORIENTED_EDGE('',*,*,#7420,.F.);
#9768=ORIENTED_EDGE('',*,*,#7416,.F.);
#9769=ORIENTED_EDGE('',*,*,#7421,.F.);
#9770=ORIENTED_EDGE('',*,*,#7422,.T.);
#9771=ORIENTED_EDGE('',*,*,#7423,.F.);
#9772=ORIENTED_EDGE('',*,*,#7419,.F.);
#9773=ORIENTED_EDGE('',*,*,#7424,.F.);
#9774=ORIENTED_EDGE('',*,*,#7425,.T.);
#9775=ORIENTED_EDGE('',*,*,#7426,.F.);
#9776=ORIENTED_EDGE('',*,*,#7422,.F.);
#9777=ORIENTED_EDGE('',*,*,#7427,.F.);
#9778=ORIENTED_EDGE('',*,*,#7428,.F.);
#9779=ORIENTED_EDGE('',*,*,#7429,.F.);
#9780=ORIENTED_EDGE('',*,*,#7425,.F.);
#9781=ORIENTED_EDGE('',*,*,#7430,.F.);
#9782=ORIENTED_EDGE('',*,*,#7431,.T.);
#9783=ORIENTED_EDGE('',*,*,#7432,.F.);
#9784=ORIENTED_EDGE('',*,*,#7431,.F.);
#9785=ORIENTED_EDGE('',*,*,#7344,.T.);
#9786=ORIENTED_EDGE('',*,*,#7433,.T.);
#9787=ORIENTED_EDGE('',*,*,#7434,.T.);
#9788=ORIENTED_EDGE('',*,*,#7435,.F.);
#9789=ORIENTED_EDGE('',*,*,#7321,.T.);
#9790=ORIENTED_EDGE('',*,*,#7436,.F.);
#9791=ORIENTED_EDGE('',*,*,#7437,.F.);
#9792=ORIENTED_EDGE('',*,*,#7438,.T.);
#9793=ORIENTED_EDGE('',*,*,#7372,.T.);
#9794=ORIENTED_EDGE('',*,*,#7439,.T.);
#9795=ORIENTED_EDGE('',*,*,#7437,.T.);
#9796=ORIENTED_EDGE('',*,*,#7440,.F.);
#9797=ORIENTED_EDGE('',*,*,#7349,.T.);
#9798=ORIENTED_EDGE('',*,*,#7441,.F.);
#9799=ORIENTED_EDGE('',*,*,#7442,.F.);
#9800=ORIENTED_EDGE('',*,*,#7443,.T.);
#9801=ORIENTED_EDGE('',*,*,#7400,.T.);
#9802=ORIENTED_EDGE('',*,*,#7444,.T.);
#9803=ORIENTED_EDGE('',*,*,#7442,.T.);
#9804=ORIENTED_EDGE('',*,*,#7445,.F.);
#9805=ORIENTED_EDGE('',*,*,#7377,.T.);
#9806=ORIENTED_EDGE('',*,*,#7446,.F.);
#9807=ORIENTED_EDGE('',*,*,#7447,.F.);
#9808=ORIENTED_EDGE('',*,*,#7448,.T.);
#9809=ORIENTED_EDGE('',*,*,#7428,.T.);
#9810=ORIENTED_EDGE('',*,*,#7449,.T.);
#9811=ORIENTED_EDGE('',*,*,#7447,.T.);
#9812=ORIENTED_EDGE('',*,*,#7450,.F.);
#9813=ORIENTED_EDGE('',*,*,#7405,.T.);
#9814=ORIENTED_EDGE('',*,*,#7451,.F.);
#9815=ORIENTED_EDGE('',*,*,#7434,.F.);
#9816=ORIENTED_EDGE('',*,*,#7452,.T.);
#9817=ORIENTED_EDGE('',*,*,#7320,.T.);
#9818=ORIENTED_EDGE('',*,*,#7324,.T.);
#9819=ORIENTED_EDGE('',*,*,#7327,.T.);
#9820=ORIENTED_EDGE('',*,*,#7330,.T.);
#9821=ORIENTED_EDGE('',*,*,#7333,.T.);
#9822=ORIENTED_EDGE('',*,*,#7336,.T.);
#9823=ORIENTED_EDGE('',*,*,#7339,.T.);
#9824=ORIENTED_EDGE('',*,*,#7342,.T.);
#9825=ORIENTED_EDGE('',*,*,#7345,.T.);
#9826=ORIENTED_EDGE('',*,*,#7435,.T.);
#9827=ORIENTED_EDGE('',*,*,#7451,.T.);
#9828=ORIENTED_EDGE('',*,*,#7404,.T.);
#9829=ORIENTED_EDGE('',*,*,#7408,.T.);
#9830=ORIENTED_EDGE('',*,*,#7411,.T.);
#9831=ORIENTED_EDGE('',*,*,#7414,.T.);
#9832=ORIENTED_EDGE('',*,*,#7417,.T.);
#9833=ORIENTED_EDGE('',*,*,#7420,.T.);
#9834=ORIENTED_EDGE('',*,*,#7423,.T.);
#9835=ORIENTED_EDGE('',*,*,#7426,.T.);
#9836=ORIENTED_EDGE('',*,*,#7429,.T.);
#9837=ORIENTED_EDGE('',*,*,#7450,.T.);
#9838=ORIENTED_EDGE('',*,*,#7446,.T.);
#9839=ORIENTED_EDGE('',*,*,#7376,.T.);
#9840=ORIENTED_EDGE('',*,*,#7380,.T.);
#9841=ORIENTED_EDGE('',*,*,#7383,.T.);
#9842=ORIENTED_EDGE('',*,*,#7386,.T.);
#9843=ORIENTED_EDGE('',*,*,#7389,.T.);
#9844=ORIENTED_EDGE('',*,*,#7392,.T.);
#9845=ORIENTED_EDGE('',*,*,#7395,.T.);
#9846=ORIENTED_EDGE('',*,*,#7398,.T.);
#9847=ORIENTED_EDGE('',*,*,#7401,.T.);
#9848=ORIENTED_EDGE('',*,*,#7445,.T.);
#9849=ORIENTED_EDGE('',*,*,#7441,.T.);
#9850=ORIENTED_EDGE('',*,*,#7348,.T.);
#9851=ORIENTED_EDGE('',*,*,#7352,.T.);
#9852=ORIENTED_EDGE('',*,*,#7355,.T.);
#9853=ORIENTED_EDGE('',*,*,#7358,.T.);
#9854=ORIENTED_EDGE('',*,*,#7361,.T.);
#9855=ORIENTED_EDGE('',*,*,#7364,.T.);
#9856=ORIENTED_EDGE('',*,*,#7367,.T.);
#9857=ORIENTED_EDGE('',*,*,#7370,.T.);
#9858=ORIENTED_EDGE('',*,*,#7373,.T.);
#9859=ORIENTED_EDGE('',*,*,#7440,.T.);
#9860=ORIENTED_EDGE('',*,*,#7436,.T.);
#9861=ORIENTED_EDGE('',*,*,#7432,.T.);
#9862=ORIENTED_EDGE('',*,*,#7318,.T.);
#9863=ORIENTED_EDGE('',*,*,#7438,.F.);
#9864=ORIENTED_EDGE('',*,*,#7439,.F.);
#9865=ORIENTED_EDGE('',*,*,#7371,.T.);
#9866=ORIENTED_EDGE('',*,*,#7368,.T.);
#9867=ORIENTED_EDGE('',*,*,#7365,.T.);
#9868=ORIENTED_EDGE('',*,*,#7362,.T.);
#9869=ORIENTED_EDGE('',*,*,#7359,.T.);
#9870=ORIENTED_EDGE('',*,*,#7356,.T.);
#9871=ORIENTED_EDGE('',*,*,#7353,.T.);
#9872=ORIENTED_EDGE('',*,*,#7350,.T.);
#9873=ORIENTED_EDGE('',*,*,#7346,.T.);
#9874=ORIENTED_EDGE('',*,*,#7443,.F.);
#9875=ORIENTED_EDGE('',*,*,#7444,.F.);
#9876=ORIENTED_EDGE('',*,*,#7399,.T.);
#9877=ORIENTED_EDGE('',*,*,#7396,.T.);
#9878=ORIENTED_EDGE('',*,*,#7393,.T.);
#9879=ORIENTED_EDGE('',*,*,#7390,.T.);
#9880=ORIENTED_EDGE('',*,*,#7387,.T.);
#9881=ORIENTED_EDGE('',*,*,#7384,.T.);
#9882=ORIENTED_EDGE('',*,*,#7381,.T.);
#9883=ORIENTED_EDGE('',*,*,#7378,.T.);
#9884=ORIENTED_EDGE('',*,*,#7374,.T.);
#9885=ORIENTED_EDGE('',*,*,#7448,.F.);
#9886=ORIENTED_EDGE('',*,*,#7449,.F.);
#9887=ORIENTED_EDGE('',*,*,#7427,.T.);
#9888=ORIENTED_EDGE('',*,*,#7424,.T.);
#9889=ORIENTED_EDGE('',*,*,#7421,.T.);
#9890=ORIENTED_EDGE('',*,*,#7418,.T.);
#9891=ORIENTED_EDGE('',*,*,#7415,.T.);
#9892=ORIENTED_EDGE('',*,*,#7412,.T.);
#9893=ORIENTED_EDGE('',*,*,#7409,.T.);
#9894=ORIENTED_EDGE('',*,*,#7406,.T.);
#9895=ORIENTED_EDGE('',*,*,#7402,.T.);
#9896=ORIENTED_EDGE('',*,*,#7452,.F.);
#9897=ORIENTED_EDGE('',*,*,#7433,.F.);
#9898=ORIENTED_EDGE('',*,*,#7343,.T.);
#9899=ORIENTED_EDGE('',*,*,#7340,.T.);
#9900=ORIENTED_EDGE('',*,*,#7337,.T.);
#9901=ORIENTED_EDGE('',*,*,#7334,.T.);
#9902=ORIENTED_EDGE('',*,*,#7331,.T.);
#9903=ORIENTED_EDGE('',*,*,#7328,.T.);
#9904=ORIENTED_EDGE('',*,*,#7325,.T.);
#9905=ORIENTED_EDGE('',*,*,#7322,.T.);
#9906=ORIENTED_EDGE('',*,*,#7430,.T.);
#9907=ORIENTED_EDGE('',*,*,#7453,.T.);
#9908=ORIENTED_EDGE('',*,*,#7454,.T.);
#9909=ORIENTED_EDGE('',*,*,#7455,.T.);
#9910=ORIENTED_EDGE('',*,*,#7456,.T.);
#9911=ORIENTED_EDGE('',*,*,#7457,.T.);
#9912=ORIENTED_EDGE('',*,*,#7458,.T.);
#9913=ORIENTED_EDGE('',*,*,#7457,.F.);
#9914=ORIENTED_EDGE('',*,*,#7459,.F.);
#9915=ORIENTED_EDGE('',*,*,#7460,.T.);
#9916=ORIENTED_EDGE('',*,*,#7461,.F.);
#9917=ORIENTED_EDGE('',*,*,#7460,.F.);
#9918=ORIENTED_EDGE('',*,*,#7462,.F.);
#9919=ORIENTED_EDGE('',*,*,#7463,.F.);
#9920=ORIENTED_EDGE('',*,*,#7464,.F.);
#9921=ORIENTED_EDGE('',*,*,#7456,.F.);
#9922=ORIENTED_EDGE('',*,*,#7465,.F.);
#9923=ORIENTED_EDGE('',*,*,#7466,.F.);
#9924=ORIENTED_EDGE('',*,*,#7462,.T.);
#9925=ORIENTED_EDGE('',*,*,#7459,.T.);
#9926=ORIENTED_EDGE('',*,*,#7458,.F.);
#9927=ORIENTED_EDGE('',*,*,#7464,.T.);
#9928=ORIENTED_EDGE('',*,*,#7467,.F.);
#9929=ORIENTED_EDGE('',*,*,#7468,.F.);
#9930=ORIENTED_EDGE('',*,*,#7469,.T.);
#9931=ORIENTED_EDGE('',*,*,#7470,.T.);
#9932=ORIENTED_EDGE('',*,*,#7471,.T.);
#9933=ORIENTED_EDGE('',*,*,#7467,.T.);
#9934=ORIENTED_EDGE('',*,*,#7463,.T.);
#9935=ORIENTED_EDGE('',*,*,#7466,.T.);
#9936=ORIENTED_EDGE('',*,*,#7453,.F.);
#9937=ORIENTED_EDGE('',*,*,#7468,.T.);
#9938=ORIENTED_EDGE('',*,*,#7471,.F.);
#9939=ORIENTED_EDGE('',*,*,#7472,.T.);
#9940=ORIENTED_EDGE('',*,*,#7473,.F.);
#9941=ORIENTED_EDGE('',*,*,#7474,.F.);
#9942=ORIENTED_EDGE('',*,*,#7470,.F.);
#9943=ORIENTED_EDGE('',*,*,#7475,.T.);
#9944=ORIENTED_EDGE('',*,*,#7476,.F.);
#9945=ORIENTED_EDGE('',*,*,#7472,.F.);
#9946=ORIENTED_EDGE('',*,*,#7454,.F.);
#9947=ORIENTED_EDGE('',*,*,#7474,.T.);
#9948=ORIENTED_EDGE('',*,*,#7477,.F.);
#9949=ORIENTED_EDGE('',*,*,#7478,.F.);
#9950=ORIENTED_EDGE('',*,*,#7455,.F.);
#9951=ORIENTED_EDGE('',*,*,#7478,.T.);
#9952=ORIENTED_EDGE('',*,*,#7479,.F.);
#9953=ORIENTED_EDGE('',*,*,#7475,.F.);
#9954=ORIENTED_EDGE('',*,*,#7469,.F.);
#9955=ORIENTED_EDGE('',*,*,#7465,.T.);
#9956=ORIENTED_EDGE('',*,*,#7479,.T.);
#9957=ORIENTED_EDGE('',*,*,#7477,.T.);
#9958=ORIENTED_EDGE('',*,*,#7473,.T.);
#9959=ORIENTED_EDGE('',*,*,#7476,.T.);
#9960=ORIENTED_EDGE('',*,*,#7461,.T.);
#9961=ORIENTED_EDGE('',*,*,#7480,.T.);
#9962=ORIENTED_EDGE('',*,*,#7481,.T.);
#9963=ORIENTED_EDGE('',*,*,#7482,.T.);
#9964=ORIENTED_EDGE('',*,*,#7481,.F.);
#9965=ORIENTED_EDGE('',*,*,#7482,.F.);
#9966=ORIENTED_EDGE('',*,*,#7483,.T.);
#9967=ORIENTED_EDGE('',*,*,#7484,.T.);
#9968=ORIENTED_EDGE('',*,*,#7483,.F.);
#9969=ORIENTED_EDGE('',*,*,#7485,.T.);
#9970=ORIENTED_EDGE('',*,*,#7480,.F.);
#9971=ORIENTED_EDGE('',*,*,#7485,.F.);
#9972=ORIENTED_EDGE('',*,*,#7486,.T.);
#9973=ORIENTED_EDGE('',*,*,#7487,.T.);
#9974=ORIENTED_EDGE('',*,*,#7486,.F.);
#9975=ORIENTED_EDGE('',*,*,#7487,.F.);
#9976=ORIENTED_EDGE('',*,*,#7484,.F.);
#9977=ORIENTED_EDGE('',*,*,#7488,.T.);
#9978=ORIENTED_EDGE('',*,*,#7489,.T.);
#9979=ORIENTED_EDGE('',*,*,#7490,.T.);
#9980=ORIENTED_EDGE('',*,*,#7491,.F.);
#9981=ORIENTED_EDGE('',*,*,#7492,.T.);
#9982=ORIENTED_EDGE('',*,*,#7493,.T.);
#9983=ORIENTED_EDGE('',*,*,#7494,.T.);
#9984=ORIENTED_EDGE('',*,*,#7489,.F.);
#9985=ORIENTED_EDGE('',*,*,#7495,.T.);
#9986=ORIENTED_EDGE('',*,*,#7496,.T.);
#9987=ORIENTED_EDGE('',*,*,#7497,.T.);
#9988=ORIENTED_EDGE('',*,*,#7493,.F.);
#9989=ORIENTED_EDGE('',*,*,#7498,.T.);
#9990=ORIENTED_EDGE('',*,*,#7499,.T.);
#9991=ORIENTED_EDGE('',*,*,#7500,.T.);
#9992=ORIENTED_EDGE('',*,*,#7496,.F.);
#9993=ORIENTED_EDGE('',*,*,#7501,.T.);
#9994=ORIENTED_EDGE('',*,*,#7502,.T.);
#9995=ORIENTED_EDGE('',*,*,#7503,.T.);
#9996=ORIENTED_EDGE('',*,*,#7499,.F.);
#9997=ORIENTED_EDGE('',*,*,#7504,.T.);
#9998=ORIENTED_EDGE('',*,*,#7491,.T.);
#9999=ORIENTED_EDGE('',*,*,#7505,.T.);
#10000=ORIENTED_EDGE('',*,*,#7502,.F.);
#10001=ORIENTED_EDGE('',*,*,#7504,.F.);
#10002=ORIENTED_EDGE('',*,*,#7501,.F.);
#10003=ORIENTED_EDGE('',*,*,#7498,.F.);
#10004=ORIENTED_EDGE('',*,*,#7495,.F.);
#10005=ORIENTED_EDGE('',*,*,#7492,.F.);
#10006=ORIENTED_EDGE('',*,*,#7488,.F.);
#10007=ORIENTED_EDGE('',*,*,#7505,.F.);
#10008=ORIENTED_EDGE('',*,*,#7490,.F.);
#10009=ORIENTED_EDGE('',*,*,#7494,.F.);
#10010=ORIENTED_EDGE('',*,*,#7497,.F.);
#10011=ORIENTED_EDGE('',*,*,#7500,.F.);
#10012=ORIENTED_EDGE('',*,*,#7503,.F.);
#10013=ORIENTED_EDGE('',*,*,#7506,.F.);
#10014=ORIENTED_EDGE('',*,*,#7507,.F.);
#10015=ORIENTED_EDGE('',*,*,#7508,.F.);
#10016=ORIENTED_EDGE('',*,*,#7509,.T.);
#10017=ORIENTED_EDGE('',*,*,#7507,.T.);
#10018=ORIENTED_EDGE('',*,*,#7509,.F.);
#10019=ORIENTED_EDGE('',*,*,#7510,.F.);
#10020=ORIENTED_EDGE('',*,*,#7511,.T.);
#10021=ORIENTED_EDGE('',*,*,#7508,.T.);
#10022=ORIENTED_EDGE('',*,*,#7511,.F.);
#10023=ORIENTED_EDGE('',*,*,#7512,.F.);
#10024=ORIENTED_EDGE('',*,*,#7513,.T.);
#10025=ORIENTED_EDGE('',*,*,#7510,.T.);
#10026=ORIENTED_EDGE('',*,*,#7513,.F.);
#10027=ORIENTED_EDGE('',*,*,#7512,.T.);
#10028=ORIENTED_EDGE('',*,*,#7514,.F.);
#10029=ORIENTED_EDGE('',*,*,#7515,.F.);
#10030=ORIENTED_EDGE('',*,*,#7516,.T.);
#10031=ORIENTED_EDGE('',*,*,#7514,.T.);
#10032=ORIENTED_EDGE('',*,*,#7516,.F.);
#10033=ORIENTED_EDGE('',*,*,#7506,.T.);
#10034=ORIENTED_EDGE('',*,*,#7517,.T.);
#10035=ORIENTED_EDGE('',*,*,#7515,.T.);
#10036=ORIENTED_EDGE('',*,*,#7517,.F.);
#10037=ORIENTED_EDGE('',*,*,#7518,.F.);
#10038=ORIENTED_EDGE('',*,*,#7519,.T.);
#10039=ORIENTED_EDGE('',*,*,#7520,.F.);
#10040=ORIENTED_EDGE('',*,*,#7519,.F.);
#10041=ORIENTED_EDGE('',*,*,#7521,.F.);
#10042=ORIENTED_EDGE('',*,*,#7522,.T.);
#10043=ORIENTED_EDGE('',*,*,#7523,.F.);
#10044=ORIENTED_EDGE('',*,*,#7522,.F.);
#10045=ORIENTED_EDGE('',*,*,#7524,.F.);
#10046=ORIENTED_EDGE('',*,*,#7525,.T.);
#10047=ORIENTED_EDGE('',*,*,#7526,.F.);
#10048=ORIENTED_EDGE('',*,*,#7525,.F.);
#10049=ORIENTED_EDGE('',*,*,#7527,.F.);
#10050=ORIENTED_EDGE('',*,*,#7528,.T.);
#10051=ORIENTED_EDGE('',*,*,#7529,.F.);
#10052=ORIENTED_EDGE('',*,*,#7528,.F.);
#10053=ORIENTED_EDGE('',*,*,#7530,.T.);
#10054=ORIENTED_EDGE('',*,*,#7531,.T.);
#10055=ORIENTED_EDGE('',*,*,#7532,.F.);
#10056=ORIENTED_EDGE('',*,*,#7533,.F.);
#10057=ORIENTED_EDGE('',*,*,#7534,.T.);
#10058=ORIENTED_EDGE('',*,*,#7533,.T.);
#10059=ORIENTED_EDGE('',*,*,#7535,.F.);
#10060=ORIENTED_EDGE('',*,*,#7536,.F.);
#10061=ORIENTED_EDGE('',*,*,#7537,.T.);
#10062=ORIENTED_EDGE('',*,*,#7536,.T.);
#10063=ORIENTED_EDGE('',*,*,#7538,.F.);
#10064=ORIENTED_EDGE('',*,*,#7539,.F.);
#10065=ORIENTED_EDGE('',*,*,#7540,.T.);
#10066=ORIENTED_EDGE('',*,*,#7539,.T.);
#10067=ORIENTED_EDGE('',*,*,#7541,.F.);
#10068=ORIENTED_EDGE('',*,*,#7531,.F.);
#10069=ORIENTED_EDGE('',*,*,#7541,.T.);
#10070=ORIENTED_EDGE('',*,*,#7538,.T.);
#10071=ORIENTED_EDGE('',*,*,#7535,.T.);
#10072=ORIENTED_EDGE('',*,*,#7532,.T.);
#10073=ORIENTED_EDGE('',*,*,#7520,.T.);
#10074=ORIENTED_EDGE('',*,*,#7523,.T.);
#10075=ORIENTED_EDGE('',*,*,#7526,.T.);
#10076=ORIENTED_EDGE('',*,*,#7529,.T.);
#10077=ORIENTED_EDGE('',*,*,#7540,.F.);
#10078=ORIENTED_EDGE('',*,*,#7530,.F.);
#10079=ORIENTED_EDGE('',*,*,#7534,.F.);
#10080=ORIENTED_EDGE('',*,*,#7537,.F.);
#10081=ORIENTED_EDGE('',*,*,#7518,.T.);
#10082=ORIENTED_EDGE('',*,*,#7521,.T.);
#10083=ORIENTED_EDGE('',*,*,#7524,.T.);
#10084=ORIENTED_EDGE('',*,*,#7527,.T.);
#10085=ORIENTED_EDGE('',*,*,#7542,.F.);
#10086=ORIENTED_EDGE('',*,*,#7543,.T.);
#10087=ORIENTED_EDGE('',*,*,#7544,.F.);
#10088=ORIENTED_EDGE('',*,*,#7543,.F.);
#10089=ORIENTED_EDGE('',*,*,#7545,.F.);
#10090=ORIENTED_EDGE('',*,*,#7546,.T.);
#10091=ORIENTED_EDGE('',*,*,#7547,.F.);
#10092=ORIENTED_EDGE('',*,*,#7546,.F.);
#10093=ORIENTED_EDGE('',*,*,#7548,.F.);
#10094=ORIENTED_EDGE('',*,*,#7549,.T.);
#10095=ORIENTED_EDGE('',*,*,#7550,.F.);
#10096=ORIENTED_EDGE('',*,*,#7549,.F.);
#10097=ORIENTED_EDGE('',*,*,#7551,.F.);
#10098=ORIENTED_EDGE('',*,*,#7552,.T.);
#10099=ORIENTED_EDGE('',*,*,#7553,.F.);
#10100=ORIENTED_EDGE('',*,*,#7552,.F.);
#10101=ORIENTED_EDGE('',*,*,#7554,.F.);
#10102=ORIENTED_EDGE('',*,*,#7555,.T.);
#10103=ORIENTED_EDGE('',*,*,#7556,.F.);
#10104=ORIENTED_EDGE('',*,*,#7555,.F.);
#10105=ORIENTED_EDGE('',*,*,#7557,.F.);
#10106=ORIENTED_EDGE('',*,*,#7558,.T.);
#10107=ORIENTED_EDGE('',*,*,#7559,.F.);
#10108=ORIENTED_EDGE('',*,*,#7558,.F.);
#10109=ORIENTED_EDGE('',*,*,#7560,.F.);
#10110=ORIENTED_EDGE('',*,*,#7561,.T.);
#10111=ORIENTED_EDGE('',*,*,#7562,.F.);
#10112=ORIENTED_EDGE('',*,*,#7561,.F.);
#10113=ORIENTED_EDGE('',*,*,#7563,.F.);
#10114=ORIENTED_EDGE('',*,*,#7564,.T.);
#10115=ORIENTED_EDGE('',*,*,#7565,.F.);
#10116=ORIENTED_EDGE('',*,*,#7564,.F.);
#10117=ORIENTED_EDGE('',*,*,#7566,.T.);
#10118=ORIENTED_EDGE('',*,*,#7567,.T.);
#10119=ORIENTED_EDGE('',*,*,#7568,.F.);
#10120=ORIENTED_EDGE('',*,*,#7569,.F.);
#10121=ORIENTED_EDGE('',*,*,#7570,.T.);
#10122=ORIENTED_EDGE('',*,*,#7569,.T.);
#10123=ORIENTED_EDGE('',*,*,#7571,.F.);
#10124=ORIENTED_EDGE('',*,*,#7572,.F.);
#10125=ORIENTED_EDGE('',*,*,#7573,.T.);
#10126=ORIENTED_EDGE('',*,*,#7572,.T.);
#10127=ORIENTED_EDGE('',*,*,#7574,.F.);
#10128=ORIENTED_EDGE('',*,*,#7575,.F.);
#10129=ORIENTED_EDGE('',*,*,#7576,.T.);
#10130=ORIENTED_EDGE('',*,*,#7575,.T.);
#10131=ORIENTED_EDGE('',*,*,#7577,.F.);
#10132=ORIENTED_EDGE('',*,*,#7567,.F.);
#10133=ORIENTED_EDGE('',*,*,#7577,.T.);
#10134=ORIENTED_EDGE('',*,*,#7574,.T.);
#10135=ORIENTED_EDGE('',*,*,#7571,.T.);
#10136=ORIENTED_EDGE('',*,*,#7568,.T.);
#10137=ORIENTED_EDGE('',*,*,#7565,.T.);
#10138=ORIENTED_EDGE('',*,*,#7562,.T.);
#10139=ORIENTED_EDGE('',*,*,#7559,.T.);
#10140=ORIENTED_EDGE('',*,*,#7556,.T.);
#10141=ORIENTED_EDGE('',*,*,#7553,.T.);
#10142=ORIENTED_EDGE('',*,*,#7550,.T.);
#10143=ORIENTED_EDGE('',*,*,#7547,.T.);
#10144=ORIENTED_EDGE('',*,*,#7544,.T.);
#10145=ORIENTED_EDGE('',*,*,#7576,.F.);
#10146=ORIENTED_EDGE('',*,*,#7566,.F.);
#10147=ORIENTED_EDGE('',*,*,#7570,.F.);
#10148=ORIENTED_EDGE('',*,*,#7573,.F.);
#10149=ORIENTED_EDGE('',*,*,#7563,.T.);
#10150=ORIENTED_EDGE('',*,*,#7560,.T.);
#10151=ORIENTED_EDGE('',*,*,#7557,.T.);
#10152=ORIENTED_EDGE('',*,*,#7554,.T.);
#10153=ORIENTED_EDGE('',*,*,#7551,.T.);
#10154=ORIENTED_EDGE('',*,*,#7548,.T.);
#10155=ORIENTED_EDGE('',*,*,#7545,.T.);
#10156=ORIENTED_EDGE('',*,*,#7542,.T.);
#10157=ORIENTED_EDGE('',*,*,#7578,.F.);
#10158=ORIENTED_EDGE('',*,*,#7579,.T.);
#10159=ORIENTED_EDGE('',*,*,#7580,.F.);
#10160=ORIENTED_EDGE('',*,*,#7579,.F.);
#10161=ORIENTED_EDGE('',*,*,#7578,.T.);
#10162=ORIENTED_EDGE('',*,*,#7581,.F.);
#10163=ORIENTED_EDGE('',*,*,#7582,.T.);
#10164=ORIENTED_EDGE('',*,*,#7583,.F.);
#10165=ORIENTED_EDGE('',*,*,#7582,.F.);
#10166=ORIENTED_EDGE('',*,*,#7581,.T.);
#10167=ORIENTED_EDGE('',*,*,#7584,.F.);
#10168=ORIENTED_EDGE('',*,*,#7585,.T.);
#10169=ORIENTED_EDGE('',*,*,#7586,.F.);
#10170=ORIENTED_EDGE('',*,*,#7585,.F.);
#10171=ORIENTED_EDGE('',*,*,#7584,.T.);
#10172=ORIENTED_EDGE('',*,*,#7587,.F.);
#10173=ORIENTED_EDGE('',*,*,#7588,.T.);
#10174=ORIENTED_EDGE('',*,*,#7589,.F.);
#10175=ORIENTED_EDGE('',*,*,#7588,.F.);
#10176=ORIENTED_EDGE('',*,*,#7587,.T.);
#10177=ORIENTED_EDGE('',*,*,#7590,.F.);
#10178=ORIENTED_EDGE('',*,*,#7591,.T.);
#10179=ORIENTED_EDGE('',*,*,#7592,.F.);
#10180=ORIENTED_EDGE('',*,*,#7591,.F.);
#10181=ORIENTED_EDGE('',*,*,#7590,.T.);
#10182=ORIENTED_EDGE('',*,*,#7593,.F.);
#10183=ORIENTED_EDGE('',*,*,#7594,.T.);
#10184=ORIENTED_EDGE('',*,*,#7595,.F.);
#10185=ORIENTED_EDGE('',*,*,#7594,.F.);
#10186=ORIENTED_EDGE('',*,*,#7593,.T.);
#10187=ORIENTED_EDGE('',*,*,#7596,.F.);
#10188=ORIENTED_EDGE('',*,*,#7597,.T.);
#10189=ORIENTED_EDGE('',*,*,#7598,.F.);
#10190=ORIENTED_EDGE('',*,*,#7597,.F.);
#10191=ORIENTED_EDGE('',*,*,#7596,.T.);
#10192=ORIENTED_EDGE('',*,*,#7599,.F.);
#10193=ORIENTED_EDGE('',*,*,#7600,.T.);
#10194=ORIENTED_EDGE('',*,*,#7601,.F.);
#10195=ORIENTED_EDGE('',*,*,#7600,.F.);
#10196=ORIENTED_EDGE('',*,*,#7602,.T.);
#10197=ORIENTED_EDGE('',*,*,#7603,.T.);
#10198=ORIENTED_EDGE('',*,*,#7604,.F.);
#10199=ORIENTED_EDGE('',*,*,#7605,.F.);
#10200=ORIENTED_EDGE('',*,*,#7606,.T.);
#10201=ORIENTED_EDGE('',*,*,#7605,.T.);
#10202=ORIENTED_EDGE('',*,*,#7607,.F.);
#10203=ORIENTED_EDGE('',*,*,#7608,.F.);
#10204=ORIENTED_EDGE('',*,*,#7592,.T.);
#10205=ORIENTED_EDGE('',*,*,#7595,.T.);
#10206=ORIENTED_EDGE('',*,*,#7598,.T.);
#10207=ORIENTED_EDGE('',*,*,#7601,.T.);
#10208=ORIENTED_EDGE('',*,*,#7609,.T.);
#10209=ORIENTED_EDGE('',*,*,#7608,.T.);
#10210=ORIENTED_EDGE('',*,*,#7610,.F.);
#10211=ORIENTED_EDGE('',*,*,#7611,.F.);
#10212=ORIENTED_EDGE('',*,*,#7612,.T.);
#10213=ORIENTED_EDGE('',*,*,#7611,.T.);
#10214=ORIENTED_EDGE('',*,*,#7613,.F.);
#10215=ORIENTED_EDGE('',*,*,#7603,.F.);
#10216=ORIENTED_EDGE('',*,*,#7599,.T.);
#10217=ORIENTED_EDGE('',*,*,#7613,.T.);
#10218=ORIENTED_EDGE('',*,*,#7610,.T.);
#10219=ORIENTED_EDGE('',*,*,#7607,.T.);
#10220=ORIENTED_EDGE('',*,*,#7604,.T.);
#10221=ORIENTED_EDGE('',*,*,#7580,.T.);
#10222=ORIENTED_EDGE('',*,*,#7583,.T.);
#10223=ORIENTED_EDGE('',*,*,#7586,.T.);
#10224=ORIENTED_EDGE('',*,*,#7589,.T.);
#10225=ORIENTED_EDGE('',*,*,#7612,.F.);
#10226=ORIENTED_EDGE('',*,*,#7602,.F.);
#10227=ORIENTED_EDGE('',*,*,#7606,.F.);
#10228=ORIENTED_EDGE('',*,*,#7609,.F.);
#10229=ORIENTED_EDGE('',*,*,#7614,.F.);
#10230=ORIENTED_EDGE('',*,*,#7615,.T.);
#10231=ORIENTED_EDGE('',*,*,#7616,.F.);
#10232=ORIENTED_EDGE('',*,*,#7617,.F.);
#10233=ORIENTED_EDGE('',*,*,#7618,.T.);
#10234=ORIENTED_EDGE('',*,*,#7619,.F.);
#10235=ORIENTED_EDGE('',*,*,#7618,.F.);
#10236=ORIENTED_EDGE('',*,*,#7620,.F.);
#10237=ORIENTED_EDGE('',*,*,#7621,.F.);
#10238=ORIENTED_EDGE('',*,*,#7615,.F.);
#10239=ORIENTED_EDGE('',*,*,#7622,.F.);
#10240=ORIENTED_EDGE('',*,*,#7623,.T.);
#10241=ORIENTED_EDGE('',*,*,#7624,.F.);
#10242=ORIENTED_EDGE('',*,*,#7625,.F.);
#10243=ORIENTED_EDGE('',*,*,#7626,.T.);
#10244=ORIENTED_EDGE('',*,*,#7627,.F.);
#10245=ORIENTED_EDGE('',*,*,#7626,.F.);
#10246=ORIENTED_EDGE('',*,*,#7628,.F.);
#10247=ORIENTED_EDGE('',*,*,#7629,.F.);
#10248=ORIENTED_EDGE('',*,*,#7623,.F.);
#10249=ORIENTED_EDGE('',*,*,#7630,.F.);
#10250=ORIENTED_EDGE('',*,*,#7631,.T.);
#10251=ORIENTED_EDGE('',*,*,#7632,.F.);
#10252=ORIENTED_EDGE('',*,*,#7633,.F.);
#10253=ORIENTED_EDGE('',*,*,#7634,.T.);
#10254=ORIENTED_EDGE('',*,*,#7635,.F.);
#10255=ORIENTED_EDGE('',*,*,#7634,.F.);
#10256=ORIENTED_EDGE('',*,*,#7636,.F.);
#10257=ORIENTED_EDGE('',*,*,#7637,.F.);
#10258=ORIENTED_EDGE('',*,*,#7631,.F.);
#10259=ORIENTED_EDGE('',*,*,#7638,.F.);
#10260=ORIENTED_EDGE('',*,*,#7639,.T.);
#10261=ORIENTED_EDGE('',*,*,#7640,.F.);
#10262=ORIENTED_EDGE('',*,*,#7641,.F.);
#10263=ORIENTED_EDGE('',*,*,#7642,.T.);
#10264=ORIENTED_EDGE('',*,*,#7643,.F.);
#10265=ORIENTED_EDGE('',*,*,#7642,.F.);
#10266=ORIENTED_EDGE('',*,*,#7644,.F.);
#10267=ORIENTED_EDGE('',*,*,#7645,.F.);
#10268=ORIENTED_EDGE('',*,*,#7639,.F.);
#10269=ORIENTED_EDGE('',*,*,#7616,.T.);
#10270=ORIENTED_EDGE('',*,*,#7614,.T.);
#10271=ORIENTED_EDGE('',*,*,#7621,.T.);
#10272=ORIENTED_EDGE('',*,*,#7646,.T.);
#10273=ORIENTED_EDGE('',*,*,#7632,.T.);
#10274=ORIENTED_EDGE('',*,*,#7630,.T.);
#10275=ORIENTED_EDGE('',*,*,#7637,.T.);
#10276=ORIENTED_EDGE('',*,*,#7647,.T.);
#10277=ORIENTED_EDGE('',*,*,#7648,.F.);
#10278=ORIENTED_EDGE('',*,*,#7649,.T.);
#10279=ORIENTED_EDGE('',*,*,#7650,.F.);
#10280=ORIENTED_EDGE('',*,*,#7651,.T.);
#10281=ORIENTED_EDGE('',*,*,#7624,.T.);
#10282=ORIENTED_EDGE('',*,*,#7622,.T.);
#10283=ORIENTED_EDGE('',*,*,#7629,.T.);
#10284=ORIENTED_EDGE('',*,*,#7652,.T.);
#10285=ORIENTED_EDGE('',*,*,#7640,.T.);
#10286=ORIENTED_EDGE('',*,*,#7638,.T.);
#10287=ORIENTED_EDGE('',*,*,#7645,.T.);
#10288=ORIENTED_EDGE('',*,*,#7653,.T.);
#10289=ORIENTED_EDGE('',*,*,#7654,.F.);
#10290=ORIENTED_EDGE('',*,*,#7655,.F.);
#10291=ORIENTED_EDGE('',*,*,#7656,.F.);
#10292=ORIENTED_EDGE('',*,*,#7657,.T.);
#10293=ORIENTED_EDGE('',*,*,#7648,.T.);
#10294=ORIENTED_EDGE('',*,*,#7658,.T.);
#10295=ORIENTED_EDGE('',*,*,#7659,.T.);
#10296=ORIENTED_EDGE('',*,*,#7660,.T.);
#10297=ORIENTED_EDGE('',*,*,#7661,.T.);
#10298=ORIENTED_EDGE('',*,*,#7662,.T.);
#10299=ORIENTED_EDGE('',*,*,#7656,.T.);
#10300=ORIENTED_EDGE('',*,*,#7663,.T.);
#10301=ORIENTED_EDGE('',*,*,#7664,.T.);
#10302=ORIENTED_EDGE('',*,*,#7665,.T.);
#10303=ORIENTED_EDGE('',*,*,#7666,.T.);
#10304=ORIENTED_EDGE('',*,*,#7667,.T.);
#10305=ORIENTED_EDGE('',*,*,#7620,.T.);
#10306=ORIENTED_EDGE('',*,*,#7617,.T.);
#10307=ORIENTED_EDGE('',*,*,#7651,.F.);
#10308=ORIENTED_EDGE('',*,*,#7668,.F.);
#10309=ORIENTED_EDGE('',*,*,#7669,.F.);
#10310=ORIENTED_EDGE('',*,*,#7658,.F.);
#10311=ORIENTED_EDGE('',*,*,#7647,.F.);
#10312=ORIENTED_EDGE('',*,*,#7636,.T.);
#10313=ORIENTED_EDGE('',*,*,#7633,.T.);
#10314=ORIENTED_EDGE('',*,*,#7646,.F.);
#10315=ORIENTED_EDGE('',*,*,#7669,.T.);
#10316=ORIENTED_EDGE('',*,*,#7670,.F.);
#10317=ORIENTED_EDGE('',*,*,#7671,.F.);
#10318=ORIENTED_EDGE('',*,*,#7659,.F.);
#10319=ORIENTED_EDGE('',*,*,#7671,.T.);
#10320=ORIENTED_EDGE('',*,*,#7672,.F.);
#10321=ORIENTED_EDGE('',*,*,#7673,.F.);
#10322=ORIENTED_EDGE('',*,*,#7660,.F.);
#10323=ORIENTED_EDGE('',*,*,#7619,.T.);
#10324=ORIENTED_EDGE('',*,*,#7627,.T.);
#10325=ORIENTED_EDGE('',*,*,#7635,.T.);
#10326=ORIENTED_EDGE('',*,*,#7643,.T.);
#10327=ORIENTED_EDGE('',*,*,#7673,.T.);
#10328=ORIENTED_EDGE('',*,*,#7674,.F.);
#10329=ORIENTED_EDGE('',*,*,#7675,.F.);
#10330=ORIENTED_EDGE('',*,*,#7661,.F.);
#10331=ORIENTED_EDGE('',*,*,#7628,.T.);
#10332=ORIENTED_EDGE('',*,*,#7625,.T.);
#10333=ORIENTED_EDGE('',*,*,#7657,.F.);
#10334=ORIENTED_EDGE('',*,*,#7662,.F.);
#10335=ORIENTED_EDGE('',*,*,#7675,.T.);
#10336=ORIENTED_EDGE('',*,*,#7676,.F.);
#10337=ORIENTED_EDGE('',*,*,#7653,.F.);
#10338=ORIENTED_EDGE('',*,*,#7644,.T.);
#10339=ORIENTED_EDGE('',*,*,#7641,.T.);
#10340=ORIENTED_EDGE('',*,*,#7652,.F.);
#10341=ORIENTED_EDGE('',*,*,#7655,.T.);
#10342=ORIENTED_EDGE('',*,*,#7677,.F.);
#10343=ORIENTED_EDGE('',*,*,#7678,.F.);
#10344=ORIENTED_EDGE('',*,*,#7663,.F.);
#10345=ORIENTED_EDGE('',*,*,#7678,.T.);
#10346=ORIENTED_EDGE('',*,*,#7679,.F.);
#10347=ORIENTED_EDGE('',*,*,#7680,.F.);
#10348=ORIENTED_EDGE('',*,*,#7664,.F.);
#10349=ORIENTED_EDGE('',*,*,#7680,.T.);
#10350=ORIENTED_EDGE('',*,*,#7681,.F.);
#10351=ORIENTED_EDGE('',*,*,#7682,.F.);
#10352=ORIENTED_EDGE('',*,*,#7665,.F.);
#10353=ORIENTED_EDGE('',*,*,#7682,.T.);
#10354=ORIENTED_EDGE('',*,*,#7683,.F.);
#10355=ORIENTED_EDGE('',*,*,#7684,.F.);
#10356=ORIENTED_EDGE('',*,*,#7666,.F.);
#10357=ORIENTED_EDGE('',*,*,#7684,.T.);
#10358=ORIENTED_EDGE('',*,*,#7685,.F.);
#10359=ORIENTED_EDGE('',*,*,#7649,.F.);
#10360=ORIENTED_EDGE('',*,*,#7667,.F.);
#10361=ORIENTED_EDGE('',*,*,#7650,.T.);
#10362=ORIENTED_EDGE('',*,*,#7685,.T.);
#10363=ORIENTED_EDGE('',*,*,#7683,.T.);
#10364=ORIENTED_EDGE('',*,*,#7681,.T.);
#10365=ORIENTED_EDGE('',*,*,#7679,.T.);
#10366=ORIENTED_EDGE('',*,*,#7677,.T.);
#10367=ORIENTED_EDGE('',*,*,#7654,.T.);
#10368=ORIENTED_EDGE('',*,*,#7676,.T.);
#10369=ORIENTED_EDGE('',*,*,#7674,.T.);
#10370=ORIENTED_EDGE('',*,*,#7672,.T.);
#10371=ORIENTED_EDGE('',*,*,#7670,.T.);
#10372=ORIENTED_EDGE('',*,*,#7668,.T.);
#10373=ORIENTED_EDGE('',*,*,#7686,.T.);
#10374=ORIENTED_EDGE('',*,*,#7687,.T.);
#10375=ORIENTED_EDGE('',*,*,#7688,.F.);
#10376=ORIENTED_EDGE('',*,*,#7689,.F.);
#10377=ORIENTED_EDGE('',*,*,#7690,.T.);
#10378=ORIENTED_EDGE('',*,*,#7689,.T.);
#10379=ORIENTED_EDGE('',*,*,#7691,.F.);
#10380=ORIENTED_EDGE('',*,*,#7692,.F.);
#10381=ORIENTED_EDGE('',*,*,#7693,.T.);
#10382=ORIENTED_EDGE('',*,*,#7692,.T.);
#10383=ORIENTED_EDGE('',*,*,#7694,.F.);
#10384=ORIENTED_EDGE('',*,*,#7695,.F.);
#10385=ORIENTED_EDGE('',*,*,#7696,.T.);
#10386=ORIENTED_EDGE('',*,*,#7695,.T.);
#10387=ORIENTED_EDGE('',*,*,#7697,.F.);
#10388=ORIENTED_EDGE('',*,*,#7698,.F.);
#10389=ORIENTED_EDGE('',*,*,#7699,.T.);
#10390=ORIENTED_EDGE('',*,*,#7698,.T.);
#10391=ORIENTED_EDGE('',*,*,#7700,.F.);
#10392=ORIENTED_EDGE('',*,*,#7701,.F.);
#10393=ORIENTED_EDGE('',*,*,#7702,.T.);
#10394=ORIENTED_EDGE('',*,*,#7701,.T.);
#10395=ORIENTED_EDGE('',*,*,#7703,.F.);
#10396=ORIENTED_EDGE('',*,*,#7704,.F.);
#10397=ORIENTED_EDGE('',*,*,#7705,.T.);
#10398=ORIENTED_EDGE('',*,*,#7704,.T.);
#10399=ORIENTED_EDGE('',*,*,#7706,.F.);
#10400=ORIENTED_EDGE('',*,*,#7707,.F.);
#10401=ORIENTED_EDGE('',*,*,#7708,.T.);
#10402=ORIENTED_EDGE('',*,*,#7707,.T.);
#10403=ORIENTED_EDGE('',*,*,#7709,.F.);
#10404=ORIENTED_EDGE('',*,*,#7687,.F.);
#10405=ORIENTED_EDGE('',*,*,#7709,.T.);
#10406=ORIENTED_EDGE('',*,*,#7706,.T.);
#10407=ORIENTED_EDGE('',*,*,#7703,.T.);
#10408=ORIENTED_EDGE('',*,*,#7700,.T.);
#10409=ORIENTED_EDGE('',*,*,#7697,.T.);
#10410=ORIENTED_EDGE('',*,*,#7694,.T.);
#10411=ORIENTED_EDGE('',*,*,#7691,.T.);
#10412=ORIENTED_EDGE('',*,*,#7688,.T.);
#10413=ORIENTED_EDGE('',*,*,#7708,.F.);
#10414=ORIENTED_EDGE('',*,*,#7686,.F.);
#10415=ORIENTED_EDGE('',*,*,#7690,.F.);
#10416=ORIENTED_EDGE('',*,*,#7693,.F.);
#10417=ORIENTED_EDGE('',*,*,#7696,.F.);
#10418=ORIENTED_EDGE('',*,*,#7699,.F.);
#10419=ORIENTED_EDGE('',*,*,#7702,.F.);
#10420=ORIENTED_EDGE('',*,*,#7705,.F.);
#10421=ORIENTED_EDGE('',*,*,#7710,.F.);
#10422=ORIENTED_EDGE('',*,*,#7711,.T.);
#10423=ORIENTED_EDGE('',*,*,#7712,.F.);
#10424=ORIENTED_EDGE('',*,*,#7713,.F.);
#10425=ORIENTED_EDGE('',*,*,#7714,.F.);
#10426=ORIENTED_EDGE('',*,*,#7713,.T.);
#10427=ORIENTED_EDGE('',*,*,#7715,.F.);
#10428=ORIENTED_EDGE('',*,*,#7716,.F.);
#10429=ORIENTED_EDGE('',*,*,#7717,.F.);
#10430=ORIENTED_EDGE('',*,*,#7716,.T.);
#10431=ORIENTED_EDGE('',*,*,#7718,.F.);
#10432=ORIENTED_EDGE('',*,*,#7719,.F.);
#10433=ORIENTED_EDGE('',*,*,#7720,.F.);
#10434=ORIENTED_EDGE('',*,*,#7719,.T.);
#10435=ORIENTED_EDGE('',*,*,#7721,.F.);
#10436=ORIENTED_EDGE('',*,*,#7722,.F.);
#10437=ORIENTED_EDGE('',*,*,#7723,.F.);
#10438=ORIENTED_EDGE('',*,*,#7722,.T.);
#10439=ORIENTED_EDGE('',*,*,#7724,.F.);
#10440=ORIENTED_EDGE('',*,*,#7725,.F.);
#10441=ORIENTED_EDGE('',*,*,#7726,.F.);
#10442=ORIENTED_EDGE('',*,*,#7725,.T.);
#10443=ORIENTED_EDGE('',*,*,#7727,.F.);
#10444=ORIENTED_EDGE('',*,*,#7728,.F.);
#10445=ORIENTED_EDGE('',*,*,#7729,.F.);
#10446=ORIENTED_EDGE('',*,*,#7728,.T.);
#10447=ORIENTED_EDGE('',*,*,#7730,.F.);
#10448=ORIENTED_EDGE('',*,*,#7731,.F.);
#10449=ORIENTED_EDGE('',*,*,#7732,.F.);
#10450=ORIENTED_EDGE('',*,*,#7731,.T.);
#10451=ORIENTED_EDGE('',*,*,#7733,.F.);
#10452=ORIENTED_EDGE('',*,*,#7711,.F.);
#10453=ORIENTED_EDGE('',*,*,#7732,.T.);
#10454=ORIENTED_EDGE('',*,*,#7710,.T.);
#10455=ORIENTED_EDGE('',*,*,#7714,.T.);
#10456=ORIENTED_EDGE('',*,*,#7717,.T.);
#10457=ORIENTED_EDGE('',*,*,#7720,.T.);
#10458=ORIENTED_EDGE('',*,*,#7723,.T.);
#10459=ORIENTED_EDGE('',*,*,#7726,.T.);
#10460=ORIENTED_EDGE('',*,*,#7729,.T.);
#10461=ORIENTED_EDGE('',*,*,#7733,.T.);
#10462=ORIENTED_EDGE('',*,*,#7730,.T.);
#10463=ORIENTED_EDGE('',*,*,#7727,.T.);
#10464=ORIENTED_EDGE('',*,*,#7724,.T.);
#10465=ORIENTED_EDGE('',*,*,#7721,.T.);
#10466=ORIENTED_EDGE('',*,*,#7718,.T.);
#10467=ORIENTED_EDGE('',*,*,#7715,.T.);
#10468=ORIENTED_EDGE('',*,*,#7712,.T.);
#10469=ORIENTED_EDGE('',*,*,#7734,.T.);
#10470=ORIENTED_EDGE('',*,*,#7735,.T.);
#10471=ORIENTED_EDGE('',*,*,#7736,.T.);
#10472=ORIENTED_EDGE('',*,*,#7735,.F.);
#10473=ORIENTED_EDGE('',*,*,#7736,.F.);
#10474=ORIENTED_EDGE('',*,*,#7737,.T.);
#10475=ORIENTED_EDGE('',*,*,#7738,.T.);
#10476=ORIENTED_EDGE('',*,*,#7737,.F.);
#10477=ORIENTED_EDGE('',*,*,#7739,.T.);
#10478=ORIENTED_EDGE('',*,*,#7734,.F.);
#10479=ORIENTED_EDGE('',*,*,#7739,.F.);
#10480=ORIENTED_EDGE('',*,*,#7740,.T.);
#10481=ORIENTED_EDGE('',*,*,#7741,.T.);
#10482=ORIENTED_EDGE('',*,*,#7740,.F.);
#10483=ORIENTED_EDGE('',*,*,#7741,.F.);
#10484=ORIENTED_EDGE('',*,*,#7738,.F.);
#10485=ORIENTED_EDGE('',*,*,#7742,.T.);
#10486=ORIENTED_EDGE('',*,*,#7743,.T.);
#10487=ORIENTED_EDGE('',*,*,#7744,.T.);
#10488=ORIENTED_EDGE('',*,*,#7745,.F.);
#10489=ORIENTED_EDGE('',*,*,#7746,.T.);
#10490=ORIENTED_EDGE('',*,*,#7747,.T.);
#10491=ORIENTED_EDGE('',*,*,#7748,.T.);
#10492=ORIENTED_EDGE('',*,*,#7743,.F.);
#10493=ORIENTED_EDGE('',*,*,#7749,.T.);
#10494=ORIENTED_EDGE('',*,*,#7750,.T.);
#10495=ORIENTED_EDGE('',*,*,#7751,.T.);
#10496=ORIENTED_EDGE('',*,*,#7747,.F.);
#10497=ORIENTED_EDGE('',*,*,#7752,.T.);
#10498=ORIENTED_EDGE('',*,*,#7753,.T.);
#10499=ORIENTED_EDGE('',*,*,#7754,.T.);
#10500=ORIENTED_EDGE('',*,*,#7750,.F.);
#10501=ORIENTED_EDGE('',*,*,#7755,.T.);
#10502=ORIENTED_EDGE('',*,*,#7756,.T.);
#10503=ORIENTED_EDGE('',*,*,#7757,.T.);
#10504=ORIENTED_EDGE('',*,*,#7753,.F.);
#10505=ORIENTED_EDGE('',*,*,#7758,.T.);
#10506=ORIENTED_EDGE('',*,*,#7745,.T.);
#10507=ORIENTED_EDGE('',*,*,#7759,.T.);
#10508=ORIENTED_EDGE('',*,*,#7756,.F.);
#10509=ORIENTED_EDGE('',*,*,#7758,.F.);
#10510=ORIENTED_EDGE('',*,*,#7755,.F.);
#10511=ORIENTED_EDGE('',*,*,#7752,.F.);
#10512=ORIENTED_EDGE('',*,*,#7749,.F.);
#10513=ORIENTED_EDGE('',*,*,#7746,.F.);
#10514=ORIENTED_EDGE('',*,*,#7742,.F.);
#10515=ORIENTED_EDGE('',*,*,#7759,.F.);
#10516=ORIENTED_EDGE('',*,*,#7744,.F.);
#10517=ORIENTED_EDGE('',*,*,#7748,.F.);
#10518=ORIENTED_EDGE('',*,*,#7751,.F.);
#10519=ORIENTED_EDGE('',*,*,#7754,.F.);
#10520=ORIENTED_EDGE('',*,*,#7757,.F.);
#10521=ORIENTED_EDGE('',*,*,#7760,.T.);
#10522=ORIENTED_EDGE('',*,*,#7761,.F.);
#10523=ORIENTED_EDGE('',*,*,#7760,.F.);
#10524=ORIENTED_EDGE('',*,*,#7762,.T.);
#10525=ORIENTED_EDGE('',*,*,#7763,.T.);
#10526=ORIENTED_EDGE('',*,*,#7762,.F.);
#10527=ORIENTED_EDGE('',*,*,#7763,.F.);
#10528=ORIENTED_EDGE('',*,*,#7764,.F.);
#10529=ORIENTED_EDGE('',*,*,#7765,.F.);
#10530=ORIENTED_EDGE('',*,*,#7766,.T.);
#10531=ORIENTED_EDGE('',*,*,#7764,.T.);
#10532=ORIENTED_EDGE('',*,*,#7766,.F.);
#10533=ORIENTED_EDGE('',*,*,#7767,.F.);
#10534=ORIENTED_EDGE('',*,*,#7768,.T.);
#10535=ORIENTED_EDGE('',*,*,#7765,.T.);
#10536=ORIENTED_EDGE('',*,*,#7768,.F.);
#10537=ORIENTED_EDGE('',*,*,#7769,.F.);
#10538=ORIENTED_EDGE('',*,*,#7770,.T.);
#10539=ORIENTED_EDGE('',*,*,#7767,.T.);
#10540=ORIENTED_EDGE('',*,*,#7770,.F.);
#10541=ORIENTED_EDGE('',*,*,#7769,.T.);
#10542=ORIENTED_EDGE('',*,*,#7771,.F.);
#10543=ORIENTED_EDGE('',*,*,#7772,.F.);
#10544=ORIENTED_EDGE('',*,*,#7773,.T.);
#10545=ORIENTED_EDGE('',*,*,#7771,.T.);
#10546=ORIENTED_EDGE('',*,*,#7773,.F.);
#10547=ORIENTED_EDGE('',*,*,#7761,.T.);
#10548=ORIENTED_EDGE('',*,*,#7774,.T.);
#10549=ORIENTED_EDGE('',*,*,#7772,.T.);
#10550=ORIENTED_EDGE('',*,*,#7774,.F.);
#10551=ORIENTED_EDGE('',*,*,#7775,.T.);
#10552=ORIENTED_EDGE('',*,*,#7776,.T.);
#10553=ORIENTED_EDGE('',*,*,#7777,.T.);
#10554=ORIENTED_EDGE('',*,*,#7778,.T.);
#10555=ORIENTED_EDGE('',*,*,#7779,.T.);
#10556=ORIENTED_EDGE('',*,*,#7780,.T.);
#10557=ORIENTED_EDGE('',*,*,#7775,.F.);
#10558=ORIENTED_EDGE('',*,*,#7781,.T.);
#10559=ORIENTED_EDGE('',*,*,#7782,.T.);
#10560=ORIENTED_EDGE('',*,*,#7783,.T.);
#10561=ORIENTED_EDGE('',*,*,#7779,.F.);
#10562=ORIENTED_EDGE('',*,*,#7784,.T.);
#10563=ORIENTED_EDGE('',*,*,#7785,.T.);
#10564=ORIENTED_EDGE('',*,*,#7786,.T.);
#10565=ORIENTED_EDGE('',*,*,#7782,.F.);
#10566=ORIENTED_EDGE('',*,*,#7787,.T.);
#10567=ORIENTED_EDGE('',*,*,#7788,.T.);
#10568=ORIENTED_EDGE('',*,*,#7789,.T.);
#10569=ORIENTED_EDGE('',*,*,#7785,.F.);
#10570=ORIENTED_EDGE('',*,*,#7790,.T.);
#10571=ORIENTED_EDGE('',*,*,#7791,.T.);
#10572=ORIENTED_EDGE('',*,*,#7792,.T.);
#10573=ORIENTED_EDGE('',*,*,#7788,.F.);
#10574=ORIENTED_EDGE('',*,*,#7793,.T.);
#10575=ORIENTED_EDGE('',*,*,#7794,.T.);
#10576=ORIENTED_EDGE('',*,*,#7795,.T.);
#10577=ORIENTED_EDGE('',*,*,#7791,.F.);
#10578=ORIENTED_EDGE('',*,*,#7796,.T.);
#10579=ORIENTED_EDGE('',*,*,#7797,.T.);
#10580=ORIENTED_EDGE('',*,*,#7798,.T.);
#10581=ORIENTED_EDGE('',*,*,#7794,.F.);
#10582=ORIENTED_EDGE('',*,*,#7799,.T.);
#10583=ORIENTED_EDGE('',*,*,#7800,.F.);
#10584=ORIENTED_EDGE('',*,*,#7801,.F.);
#10585=ORIENTED_EDGE('',*,*,#7802,.T.);
#10586=ORIENTED_EDGE('',*,*,#7803,.T.);
#10587=ORIENTED_EDGE('',*,*,#7804,.T.);
#10588=ORIENTED_EDGE('',*,*,#7805,.F.);
#10589=ORIENTED_EDGE('',*,*,#7806,.F.);
#10590=ORIENTED_EDGE('',*,*,#7807,.T.);
#10591=ORIENTED_EDGE('',*,*,#7808,.T.);
#10592=ORIENTED_EDGE('',*,*,#7803,.F.);
#10593=ORIENTED_EDGE('',*,*,#7809,.F.);
#10594=ORIENTED_EDGE('',*,*,#7810,.T.);
#10595=ORIENTED_EDGE('',*,*,#7811,.T.);
#10596=ORIENTED_EDGE('',*,*,#7807,.F.);
#10597=ORIENTED_EDGE('',*,*,#7812,.F.);
#10598=ORIENTED_EDGE('',*,*,#7813,.T.);
#10599=ORIENTED_EDGE('',*,*,#7814,.T.);
#10600=ORIENTED_EDGE('',*,*,#7810,.F.);
#10601=ORIENTED_EDGE('',*,*,#7815,.F.);
#10602=ORIENTED_EDGE('',*,*,#7816,.T.);
#10603=ORIENTED_EDGE('',*,*,#7817,.T.);
#10604=ORIENTED_EDGE('',*,*,#7813,.F.);
#10605=ORIENTED_EDGE('',*,*,#7818,.F.);
#10606=ORIENTED_EDGE('',*,*,#7819,.T.);
#10607=ORIENTED_EDGE('',*,*,#7820,.T.);
#10608=ORIENTED_EDGE('',*,*,#7816,.F.);
#10609=ORIENTED_EDGE('',*,*,#7821,.F.);
#10610=ORIENTED_EDGE('',*,*,#7822,.T.);
#10611=ORIENTED_EDGE('',*,*,#7823,.T.);
#10612=ORIENTED_EDGE('',*,*,#7819,.F.);
#10613=ORIENTED_EDGE('',*,*,#7824,.F.);
#10614=ORIENTED_EDGE('',*,*,#7825,.T.);
#10615=ORIENTED_EDGE('',*,*,#7826,.T.);
#10616=ORIENTED_EDGE('',*,*,#7822,.F.);
#10617=ORIENTED_EDGE('',*,*,#7827,.F.);
#10618=ORIENTED_EDGE('',*,*,#7828,.F.);
#10619=ORIENTED_EDGE('',*,*,#7829,.F.);
#10620=ORIENTED_EDGE('',*,*,#7830,.F.);
#10621=ORIENTED_EDGE('',*,*,#7831,.T.);
#10622=ORIENTED_EDGE('',*,*,#7828,.T.);
#10623=ORIENTED_EDGE('',*,*,#7832,.T.);
#10624=ORIENTED_EDGE('',*,*,#7825,.F.);
#10625=ORIENTED_EDGE('',*,*,#7833,.F.);
#10626=ORIENTED_EDGE('',*,*,#7834,.F.);
#10627=ORIENTED_EDGE('',*,*,#7804,.F.);
#10628=ORIENTED_EDGE('',*,*,#7808,.F.);
#10629=ORIENTED_EDGE('',*,*,#7811,.F.);
#10630=ORIENTED_EDGE('',*,*,#7814,.F.);
#10631=ORIENTED_EDGE('',*,*,#7817,.F.);
#10632=ORIENTED_EDGE('',*,*,#7820,.F.);
#10633=ORIENTED_EDGE('',*,*,#7823,.F.);
#10634=ORIENTED_EDGE('',*,*,#7826,.F.);
#10635=ORIENTED_EDGE('',*,*,#7832,.F.);
#10636=ORIENTED_EDGE('',*,*,#7831,.F.);
#10637=ORIENTED_EDGE('',*,*,#7835,.F.);
#10638=ORIENTED_EDGE('',*,*,#7776,.F.);
#10639=ORIENTED_EDGE('',*,*,#7780,.F.);
#10640=ORIENTED_EDGE('',*,*,#7783,.F.);
#10641=ORIENTED_EDGE('',*,*,#7786,.F.);
#10642=ORIENTED_EDGE('',*,*,#7789,.F.);
#10643=ORIENTED_EDGE('',*,*,#7792,.F.);
#10644=ORIENTED_EDGE('',*,*,#7795,.F.);
#10645=ORIENTED_EDGE('',*,*,#7798,.F.);
#10646=ORIENTED_EDGE('',*,*,#7836,.F.);
#10647=ORIENTED_EDGE('',*,*,#7802,.F.);
#10648=ORIENTED_EDGE('',*,*,#7837,.F.);
#10649=ORIENTED_EDGE('',*,*,#7838,.F.);
#10650=ORIENTED_EDGE('',*,*,#7799,.F.);
#10651=ORIENTED_EDGE('',*,*,#7796,.F.);
#10652=ORIENTED_EDGE('',*,*,#7793,.F.);
#10653=ORIENTED_EDGE('',*,*,#7790,.F.);
#10654=ORIENTED_EDGE('',*,*,#7787,.F.);
#10655=ORIENTED_EDGE('',*,*,#7784,.F.);
#10656=ORIENTED_EDGE('',*,*,#7781,.F.);
#10657=ORIENTED_EDGE('',*,*,#7778,.F.);
#10658=ORIENTED_EDGE('',*,*,#7839,.F.);
#10659=ORIENTED_EDGE('',*,*,#7829,.T.);
#10660=ORIENTED_EDGE('',*,*,#7833,.T.);
#10661=ORIENTED_EDGE('',*,*,#7827,.T.);
#10662=ORIENTED_EDGE('',*,*,#7824,.T.);
#10663=ORIENTED_EDGE('',*,*,#7821,.T.);
#10664=ORIENTED_EDGE('',*,*,#7818,.T.);
#10665=ORIENTED_EDGE('',*,*,#7815,.T.);
#10666=ORIENTED_EDGE('',*,*,#7812,.T.);
#10667=ORIENTED_EDGE('',*,*,#7809,.T.);
#10668=ORIENTED_EDGE('',*,*,#7806,.T.);
#10669=ORIENTED_EDGE('',*,*,#7840,.T.);
#10670=ORIENTED_EDGE('',*,*,#7841,.T.);
#10671=ORIENTED_EDGE('',*,*,#7837,.T.);
#10672=ORIENTED_EDGE('',*,*,#7805,.T.);
#10673=ORIENTED_EDGE('',*,*,#7834,.T.);
#10674=ORIENTED_EDGE('',*,*,#7801,.T.);
#10675=ORIENTED_EDGE('',*,*,#7842,.T.);
#10676=ORIENTED_EDGE('',*,*,#7843,.T.);
#10677=ORIENTED_EDGE('',*,*,#7844,.T.);
#10678=ORIENTED_EDGE('',*,*,#7845,.T.);
#10679=ORIENTED_EDGE('',*,*,#7846,.F.);
#10680=ORIENTED_EDGE('',*,*,#7847,.T.);
#10681=ORIENTED_EDGE('',*,*,#7845,.F.);
#10682=ORIENTED_EDGE('',*,*,#7847,.F.);
#10683=ORIENTED_EDGE('',*,*,#7848,.F.);
#10684=ORIENTED_EDGE('',*,*,#7849,.T.);
#10685=ORIENTED_EDGE('',*,*,#7844,.F.);
#10686=ORIENTED_EDGE('',*,*,#7849,.F.);
#10687=ORIENTED_EDGE('',*,*,#7850,.F.);
#10688=ORIENTED_EDGE('',*,*,#7851,.T.);
#10689=ORIENTED_EDGE('',*,*,#7843,.F.);
#10690=ORIENTED_EDGE('',*,*,#7851,.F.);
#10691=ORIENTED_EDGE('',*,*,#7852,.F.);
#10692=ORIENTED_EDGE('',*,*,#7853,.F.);
#10693=ORIENTED_EDGE('',*,*,#7840,.F.);
#10694=ORIENTED_EDGE('',*,*,#7854,.F.);
#10695=ORIENTED_EDGE('',*,*,#7852,.T.);
#10696=ORIENTED_EDGE('',*,*,#7855,.F.);
#10697=ORIENTED_EDGE('',*,*,#7846,.T.);
#10698=ORIENTED_EDGE('',*,*,#7848,.T.);
#10699=ORIENTED_EDGE('',*,*,#7850,.T.);
#10700=ORIENTED_EDGE('',*,*,#7856,.T.);
#10701=ORIENTED_EDGE('',*,*,#7854,.T.);
#10702=ORIENTED_EDGE('',*,*,#7841,.F.);
#10703=ORIENTED_EDGE('',*,*,#7853,.T.);
#10704=ORIENTED_EDGE('',*,*,#7855,.T.);
#10705=ORIENTED_EDGE('',*,*,#7800,.T.);
#10706=ORIENTED_EDGE('',*,*,#7836,.T.);
#10707=ORIENTED_EDGE('',*,*,#7797,.F.);
#10708=ORIENTED_EDGE('',*,*,#7838,.T.);
#10709=ORIENTED_EDGE('',*,*,#7842,.F.);
#10710=ORIENTED_EDGE('',*,*,#7856,.F.);
#10711=ORIENTED_EDGE('',*,*,#7857,.T.);
#10712=ORIENTED_EDGE('',*,*,#7858,.T.);
#10713=ORIENTED_EDGE('',*,*,#7857,.F.);
#10714=ORIENTED_EDGE('',*,*,#7858,.F.);
#10715=ORIENTED_EDGE('',*,*,#7839,.T.);
#10716=ORIENTED_EDGE('',*,*,#7777,.F.);
#10717=ORIENTED_EDGE('',*,*,#7835,.T.);
#10718=ORIENTED_EDGE('',*,*,#7830,.T.);
#10719=ORIENTED_EDGE('',*,*,#7859,.F.);
#10720=ORIENTED_EDGE('',*,*,#7860,.F.);
#10721=ORIENTED_EDGE('',*,*,#7861,.T.);
#10722=ORIENTED_EDGE('',*,*,#7859,.T.);
#10723=ORIENTED_EDGE('',*,*,#7861,.F.);
#10724=ORIENTED_EDGE('',*,*,#7862,.F.);
#10725=ORIENTED_EDGE('',*,*,#7863,.T.);
#10726=ORIENTED_EDGE('',*,*,#7860,.T.);
#10727=ORIENTED_EDGE('',*,*,#7863,.F.);
#10728=ORIENTED_EDGE('',*,*,#7864,.F.);
#10729=ORIENTED_EDGE('',*,*,#7865,.T.);
#10730=ORIENTED_EDGE('',*,*,#7862,.T.);
#10731=ORIENTED_EDGE('',*,*,#7865,.F.);
#10732=ORIENTED_EDGE('',*,*,#7864,.T.);
#10733=ORIENTED_EDGE('',*,*,#7866,.F.);
#10734=ORIENTED_EDGE('',*,*,#7867,.F.);
#10735=ORIENTED_EDGE('',*,*,#7868,.T.);
#10736=ORIENTED_EDGE('',*,*,#7866,.T.);
#10737=ORIENTED_EDGE('',*,*,#7868,.F.);
#10738=ORIENTED_EDGE('',*,*,#7869,.F.);
#10739=ORIENTED_EDGE('',*,*,#7870,.T.);
#10740=ORIENTED_EDGE('',*,*,#7867,.T.);
#10741=ORIENTED_EDGE('',*,*,#7870,.F.);
#10742=ORIENTED_EDGE('',*,*,#7871,.F.);
#10743=ORIENTED_EDGE('',*,*,#7872,.T.);
#10744=ORIENTED_EDGE('',*,*,#7869,.T.);
#10745=ORIENTED_EDGE('',*,*,#7872,.F.);
#10746=ORIENTED_EDGE('',*,*,#7871,.T.);
#10747=ORIENTED_EDGE('',*,*,#7873,.T.);
#10748=ORIENTED_EDGE('',*,*,#7874,.T.);
#10749=ORIENTED_EDGE('',*,*,#7875,.T.);
#10750=ORIENTED_EDGE('',*,*,#7876,.F.);
#10751=ORIENTED_EDGE('',*,*,#7877,.T.);
#10752=ORIENTED_EDGE('',*,*,#7878,.T.);
#10753=ORIENTED_EDGE('',*,*,#7879,.T.);
#10754=ORIENTED_EDGE('',*,*,#7874,.F.);
#10755=ORIENTED_EDGE('',*,*,#7880,.T.);
#10756=ORIENTED_EDGE('',*,*,#7881,.T.);
#10757=ORIENTED_EDGE('',*,*,#7882,.T.);
#10758=ORIENTED_EDGE('',*,*,#7878,.F.);
#10759=ORIENTED_EDGE('',*,*,#7883,.T.);
#10760=ORIENTED_EDGE('',*,*,#7884,.T.);
#10761=ORIENTED_EDGE('',*,*,#7885,.T.);
#10762=ORIENTED_EDGE('',*,*,#7881,.F.);
#10763=ORIENTED_EDGE('',*,*,#7886,.T.);
#10764=ORIENTED_EDGE('',*,*,#7887,.T.);
#10765=ORIENTED_EDGE('',*,*,#7888,.T.);
#10766=ORIENTED_EDGE('',*,*,#7884,.F.);
#10767=ORIENTED_EDGE('',*,*,#7889,.T.);
#10768=ORIENTED_EDGE('',*,*,#7876,.T.);
#10769=ORIENTED_EDGE('',*,*,#7890,.T.);
#10770=ORIENTED_EDGE('',*,*,#7887,.F.);
#10771=ORIENTED_EDGE('',*,*,#7889,.F.);
#10772=ORIENTED_EDGE('',*,*,#7886,.F.);
#10773=ORIENTED_EDGE('',*,*,#7883,.F.);
#10774=ORIENTED_EDGE('',*,*,#7880,.F.);
#10775=ORIENTED_EDGE('',*,*,#7877,.F.);
#10776=ORIENTED_EDGE('',*,*,#7873,.F.);
#10777=ORIENTED_EDGE('',*,*,#7890,.F.);
#10778=ORIENTED_EDGE('',*,*,#7875,.F.);
#10779=ORIENTED_EDGE('',*,*,#7879,.F.);
#10780=ORIENTED_EDGE('',*,*,#7882,.F.);
#10781=ORIENTED_EDGE('',*,*,#7885,.F.);
#10782=ORIENTED_EDGE('',*,*,#7888,.F.);
#10783=ORIENTED_EDGE('',*,*,#7891,.F.);
#10784=ORIENTED_EDGE('',*,*,#7892,.F.);
#10785=ORIENTED_EDGE('',*,*,#7893,.T.);
#10786=ORIENTED_EDGE('',*,*,#7891,.T.);
#10787=ORIENTED_EDGE('',*,*,#7893,.F.);
#10788=ORIENTED_EDGE('',*,*,#7894,.F.);
#10789=ORIENTED_EDGE('',*,*,#7895,.T.);
#10790=ORIENTED_EDGE('',*,*,#7892,.T.);
#10791=ORIENTED_EDGE('',*,*,#7895,.F.);
#10792=ORIENTED_EDGE('',*,*,#7896,.F.);
#10793=ORIENTED_EDGE('',*,*,#7897,.T.);
#10794=ORIENTED_EDGE('',*,*,#7894,.T.);
#10795=ORIENTED_EDGE('',*,*,#7897,.F.);
#10796=ORIENTED_EDGE('',*,*,#7896,.T.);
#10797=ORIENTED_EDGE('',*,*,#7898,.F.);
#10798=ORIENTED_EDGE('',*,*,#7899,.F.);
#10799=ORIENTED_EDGE('',*,*,#7900,.T.);
#10800=ORIENTED_EDGE('',*,*,#7898,.T.);
#10801=ORIENTED_EDGE('',*,*,#7900,.F.);
#10802=ORIENTED_EDGE('',*,*,#7901,.F.);
#10803=ORIENTED_EDGE('',*,*,#7902,.T.);
#10804=ORIENTED_EDGE('',*,*,#7899,.T.);
#10805=ORIENTED_EDGE('',*,*,#7902,.F.);
#10806=ORIENTED_EDGE('',*,*,#7903,.F.);
#10807=ORIENTED_EDGE('',*,*,#7904,.T.);
#10808=ORIENTED_EDGE('',*,*,#7901,.T.);
#10809=ORIENTED_EDGE('',*,*,#7904,.F.);
#10810=ORIENTED_EDGE('',*,*,#7903,.T.);
#10811=ORIENTED_EDGE('',*,*,#7905,.T.);
#10812=ORIENTED_EDGE('',*,*,#7906,.T.);
#10813=ORIENTED_EDGE('',*,*,#7907,.T.);
#10814=ORIENTED_EDGE('',*,*,#7908,.F.);
#10815=ORIENTED_EDGE('',*,*,#7909,.T.);
#10816=ORIENTED_EDGE('',*,*,#7910,.T.);
#10817=ORIENTED_EDGE('',*,*,#7911,.T.);
#10818=ORIENTED_EDGE('',*,*,#7906,.F.);
#10819=ORIENTED_EDGE('',*,*,#7912,.T.);
#10820=ORIENTED_EDGE('',*,*,#7913,.T.);
#10821=ORIENTED_EDGE('',*,*,#7914,.T.);
#10822=ORIENTED_EDGE('',*,*,#7910,.F.);
#10823=ORIENTED_EDGE('',*,*,#7915,.T.);
#10824=ORIENTED_EDGE('',*,*,#7916,.T.);
#10825=ORIENTED_EDGE('',*,*,#7917,.T.);
#10826=ORIENTED_EDGE('',*,*,#7913,.F.);
#10827=ORIENTED_EDGE('',*,*,#7918,.T.);
#10828=ORIENTED_EDGE('',*,*,#7919,.T.);
#10829=ORIENTED_EDGE('',*,*,#7920,.T.);
#10830=ORIENTED_EDGE('',*,*,#7916,.F.);
#10831=ORIENTED_EDGE('',*,*,#7921,.T.);
#10832=ORIENTED_EDGE('',*,*,#7908,.T.);
#10833=ORIENTED_EDGE('',*,*,#7922,.T.);
#10834=ORIENTED_EDGE('',*,*,#7919,.F.);
#10835=ORIENTED_EDGE('',*,*,#7921,.F.);
#10836=ORIENTED_EDGE('',*,*,#7918,.F.);
#10837=ORIENTED_EDGE('',*,*,#7915,.F.);
#10838=ORIENTED_EDGE('',*,*,#7912,.F.);
#10839=ORIENTED_EDGE('',*,*,#7909,.F.);
#10840=ORIENTED_EDGE('',*,*,#7905,.F.);
#10841=ORIENTED_EDGE('',*,*,#7922,.F.);
#10842=ORIENTED_EDGE('',*,*,#7907,.F.);
#10843=ORIENTED_EDGE('',*,*,#7911,.F.);
#10844=ORIENTED_EDGE('',*,*,#7914,.F.);
#10845=ORIENTED_EDGE('',*,*,#7917,.F.);
#10846=ORIENTED_EDGE('',*,*,#7920,.F.);
#10847=ORIENTED_EDGE('',*,*,#7923,.F.);
#10848=ORIENTED_EDGE('',*,*,#7924,.T.);
#10849=ORIENTED_EDGE('',*,*,#7925,.T.);
#10850=ORIENTED_EDGE('',*,*,#7926,.T.);
#10851=ORIENTED_EDGE('',*,*,#7927,.F.);
#10852=ORIENTED_EDGE('',*,*,#7928,.T.);
#10853=ORIENTED_EDGE('',*,*,#7923,.T.);
#10854=ORIENTED_EDGE('',*,*,#7929,.T.);
#10855=ORIENTED_EDGE('',*,*,#7930,.F.);
#10856=ORIENTED_EDGE('',*,*,#7931,.T.);
#10857=ORIENTED_EDGE('',*,*,#7927,.T.);
#10858=ORIENTED_EDGE('',*,*,#7932,.T.);
#10859=ORIENTED_EDGE('',*,*,#7933,.F.);
#10860=ORIENTED_EDGE('',*,*,#7934,.T.);
#10861=ORIENTED_EDGE('',*,*,#7930,.T.);
#10862=ORIENTED_EDGE('',*,*,#7935,.T.);
#10863=ORIENTED_EDGE('',*,*,#7936,.F.);
#10864=ORIENTED_EDGE('',*,*,#7937,.T.);
#10865=ORIENTED_EDGE('',*,*,#7933,.T.);
#10866=ORIENTED_EDGE('',*,*,#7938,.T.);
#10867=ORIENTED_EDGE('',*,*,#7939,.F.);
#10868=ORIENTED_EDGE('',*,*,#7940,.T.);
#10869=ORIENTED_EDGE('',*,*,#7936,.T.);
#10870=ORIENTED_EDGE('',*,*,#7941,.T.);
#10871=ORIENTED_EDGE('',*,*,#7942,.F.);
#10872=ORIENTED_EDGE('',*,*,#7943,.T.);
#10873=ORIENTED_EDGE('',*,*,#7939,.T.);
#10874=ORIENTED_EDGE('',*,*,#7944,.T.);
#10875=ORIENTED_EDGE('',*,*,#7945,.F.);
#10876=ORIENTED_EDGE('',*,*,#7946,.T.);
#10877=ORIENTED_EDGE('',*,*,#7942,.T.);
#10878=ORIENTED_EDGE('',*,*,#7947,.T.);
#10879=ORIENTED_EDGE('',*,*,#7948,.F.);
#10880=ORIENTED_EDGE('',*,*,#7949,.T.);
#10881=ORIENTED_EDGE('',*,*,#7945,.T.);
#10882=ORIENTED_EDGE('',*,*,#7950,.T.);
#10883=ORIENTED_EDGE('',*,*,#7951,.F.);
#10884=ORIENTED_EDGE('',*,*,#7952,.T.);
#10885=ORIENTED_EDGE('',*,*,#7948,.T.);
#10886=ORIENTED_EDGE('',*,*,#7953,.T.);
#10887=ORIENTED_EDGE('',*,*,#7954,.F.);
#10888=ORIENTED_EDGE('',*,*,#7955,.T.);
#10889=ORIENTED_EDGE('',*,*,#7951,.T.);
#10890=ORIENTED_EDGE('',*,*,#7956,.T.);
#10891=ORIENTED_EDGE('',*,*,#7957,.F.);
#10892=ORIENTED_EDGE('',*,*,#7958,.T.);
#10893=ORIENTED_EDGE('',*,*,#7954,.T.);
#10894=ORIENTED_EDGE('',*,*,#7959,.T.);
#10895=ORIENTED_EDGE('',*,*,#7960,.F.);
#10896=ORIENTED_EDGE('',*,*,#7961,.T.);
#10897=ORIENTED_EDGE('',*,*,#7957,.T.);
#10898=ORIENTED_EDGE('',*,*,#7962,.T.);
#10899=ORIENTED_EDGE('',*,*,#7963,.F.);
#10900=ORIENTED_EDGE('',*,*,#7964,.T.);
#10901=ORIENTED_EDGE('',*,*,#7960,.T.);
#10902=ORIENTED_EDGE('',*,*,#7965,.T.);
#10903=ORIENTED_EDGE('',*,*,#7966,.F.);
#10904=ORIENTED_EDGE('',*,*,#7967,.T.);
#10905=ORIENTED_EDGE('',*,*,#7963,.T.);
#10906=ORIENTED_EDGE('',*,*,#7968,.T.);
#10907=ORIENTED_EDGE('',*,*,#7969,.F.);
#10908=ORIENTED_EDGE('',*,*,#7970,.T.);
#10909=ORIENTED_EDGE('',*,*,#7966,.T.);
#10910=ORIENTED_EDGE('',*,*,#7971,.T.);
#10911=ORIENTED_EDGE('',*,*,#7972,.F.);
#10912=ORIENTED_EDGE('',*,*,#7973,.T.);
#10913=ORIENTED_EDGE('',*,*,#7969,.T.);
#10914=ORIENTED_EDGE('',*,*,#7974,.T.);
#10915=ORIENTED_EDGE('',*,*,#7975,.F.);
#10916=ORIENTED_EDGE('',*,*,#7976,.T.);
#10917=ORIENTED_EDGE('',*,*,#7972,.T.);
#10918=ORIENTED_EDGE('',*,*,#7977,.T.);
#10919=ORIENTED_EDGE('',*,*,#7978,.F.);
#10920=ORIENTED_EDGE('',*,*,#7979,.T.);
#10921=ORIENTED_EDGE('',*,*,#7975,.T.);
#10922=ORIENTED_EDGE('',*,*,#7980,.T.);
#10923=ORIENTED_EDGE('',*,*,#7981,.F.);
#10924=ORIENTED_EDGE('',*,*,#7982,.T.);
#10925=ORIENTED_EDGE('',*,*,#7978,.T.);
#10926=ORIENTED_EDGE('',*,*,#7983,.T.);
#10927=ORIENTED_EDGE('',*,*,#7984,.F.);
#10928=ORIENTED_EDGE('',*,*,#7985,.T.);
#10929=ORIENTED_EDGE('',*,*,#7981,.T.);
#10930=ORIENTED_EDGE('',*,*,#7986,.T.);
#10931=ORIENTED_EDGE('',*,*,#7987,.F.);
#10932=ORIENTED_EDGE('',*,*,#7988,.T.);
#10933=ORIENTED_EDGE('',*,*,#7984,.T.);
#10934=ORIENTED_EDGE('',*,*,#7989,.T.);
#10935=ORIENTED_EDGE('',*,*,#7990,.F.);
#10936=ORIENTED_EDGE('',*,*,#7991,.T.);
#10937=ORIENTED_EDGE('',*,*,#7987,.T.);
#10938=ORIENTED_EDGE('',*,*,#7992,.T.);
#10939=ORIENTED_EDGE('',*,*,#7993,.F.);
#10940=ORIENTED_EDGE('',*,*,#7994,.T.);
#10941=ORIENTED_EDGE('',*,*,#7990,.T.);
#10942=ORIENTED_EDGE('',*,*,#7995,.T.);
#10943=ORIENTED_EDGE('',*,*,#7996,.F.);
#10944=ORIENTED_EDGE('',*,*,#7997,.T.);
#10945=ORIENTED_EDGE('',*,*,#7993,.T.);
#10946=ORIENTED_EDGE('',*,*,#7998,.T.);
#10947=ORIENTED_EDGE('',*,*,#7999,.F.);
#10948=ORIENTED_EDGE('',*,*,#8000,.T.);
#10949=ORIENTED_EDGE('',*,*,#7996,.T.);
#10950=ORIENTED_EDGE('',*,*,#8001,.T.);
#10951=ORIENTED_EDGE('',*,*,#8002,.F.);
#10952=ORIENTED_EDGE('',*,*,#8003,.T.);
#10953=ORIENTED_EDGE('',*,*,#7999,.T.);
#10954=ORIENTED_EDGE('',*,*,#8004,.T.);
#10955=ORIENTED_EDGE('',*,*,#8005,.F.);
#10956=ORIENTED_EDGE('',*,*,#8006,.T.);
#10957=ORIENTED_EDGE('',*,*,#8002,.T.);
#10958=ORIENTED_EDGE('',*,*,#8007,.T.);
#10959=ORIENTED_EDGE('',*,*,#8008,.F.);
#10960=ORIENTED_EDGE('',*,*,#8009,.T.);
#10961=ORIENTED_EDGE('',*,*,#8005,.T.);
#10962=ORIENTED_EDGE('',*,*,#8010,.T.);
#10963=ORIENTED_EDGE('',*,*,#8011,.F.);
#10964=ORIENTED_EDGE('',*,*,#8012,.T.);
#10965=ORIENTED_EDGE('',*,*,#8008,.T.);
#10966=ORIENTED_EDGE('',*,*,#8013,.T.);
#10967=ORIENTED_EDGE('',*,*,#8014,.F.);
#10968=ORIENTED_EDGE('',*,*,#8015,.T.);
#10969=ORIENTED_EDGE('',*,*,#8011,.T.);
#10970=ORIENTED_EDGE('',*,*,#8016,.T.);
#10971=ORIENTED_EDGE('',*,*,#8017,.F.);
#10972=ORIENTED_EDGE('',*,*,#8018,.T.);
#10973=ORIENTED_EDGE('',*,*,#8014,.T.);
#10974=ORIENTED_EDGE('',*,*,#8019,.T.);
#10975=ORIENTED_EDGE('',*,*,#8020,.F.);
#10976=ORIENTED_EDGE('',*,*,#8021,.T.);
#10977=ORIENTED_EDGE('',*,*,#8017,.T.);
#10978=ORIENTED_EDGE('',*,*,#8022,.T.);
#10979=ORIENTED_EDGE('',*,*,#8023,.F.);
#10980=ORIENTED_EDGE('',*,*,#8024,.T.);
#10981=ORIENTED_EDGE('',*,*,#8020,.T.);
#10982=ORIENTED_EDGE('',*,*,#8025,.T.);
#10983=ORIENTED_EDGE('',*,*,#8026,.F.);
#10984=ORIENTED_EDGE('',*,*,#8027,.T.);
#10985=ORIENTED_EDGE('',*,*,#8023,.T.);
#10986=ORIENTED_EDGE('',*,*,#8028,.T.);
#10987=ORIENTED_EDGE('',*,*,#8029,.F.);
#10988=ORIENTED_EDGE('',*,*,#8030,.T.);
#10989=ORIENTED_EDGE('',*,*,#8026,.T.);
#10990=ORIENTED_EDGE('',*,*,#8031,.T.);
#10991=ORIENTED_EDGE('',*,*,#8032,.F.);
#10992=ORIENTED_EDGE('',*,*,#8033,.T.);
#10993=ORIENTED_EDGE('',*,*,#8029,.T.);
#10994=ORIENTED_EDGE('',*,*,#8034,.T.);
#10995=ORIENTED_EDGE('',*,*,#8035,.F.);
#10996=ORIENTED_EDGE('',*,*,#8036,.T.);
#10997=ORIENTED_EDGE('',*,*,#8032,.T.);
#10998=ORIENTED_EDGE('',*,*,#8037,.T.);
#10999=ORIENTED_EDGE('',*,*,#8038,.F.);
#11000=ORIENTED_EDGE('',*,*,#8039,.T.);
#11001=ORIENTED_EDGE('',*,*,#8035,.T.);
#11002=ORIENTED_EDGE('',*,*,#8040,.T.);
#11003=ORIENTED_EDGE('',*,*,#8041,.F.);
#11004=ORIENTED_EDGE('',*,*,#8042,.T.);
#11005=ORIENTED_EDGE('',*,*,#8038,.T.);
#11006=ORIENTED_EDGE('',*,*,#8043,.T.);
#11007=ORIENTED_EDGE('',*,*,#8044,.F.);
#11008=ORIENTED_EDGE('',*,*,#8045,.T.);
#11009=ORIENTED_EDGE('',*,*,#8041,.T.);
#11010=ORIENTED_EDGE('',*,*,#8046,.T.);
#11011=ORIENTED_EDGE('',*,*,#8047,.F.);
#11012=ORIENTED_EDGE('',*,*,#8048,.T.);
#11013=ORIENTED_EDGE('',*,*,#8044,.T.);
#11014=ORIENTED_EDGE('',*,*,#8049,.T.);
#11015=ORIENTED_EDGE('',*,*,#8050,.F.);
#11016=ORIENTED_EDGE('',*,*,#8051,.T.);
#11017=ORIENTED_EDGE('',*,*,#8047,.T.);
#11018=ORIENTED_EDGE('',*,*,#8052,.T.);
#11019=ORIENTED_EDGE('',*,*,#8053,.F.);
#11020=ORIENTED_EDGE('',*,*,#8054,.T.);
#11021=ORIENTED_EDGE('',*,*,#8050,.T.);
#11022=ORIENTED_EDGE('',*,*,#8055,.T.);
#11023=ORIENTED_EDGE('',*,*,#8056,.F.);
#11024=ORIENTED_EDGE('',*,*,#8057,.T.);
#11025=ORIENTED_EDGE('',*,*,#8053,.T.);
#11026=ORIENTED_EDGE('',*,*,#8058,.T.);
#11027=ORIENTED_EDGE('',*,*,#8059,.F.);
#11028=ORIENTED_EDGE('',*,*,#8060,.T.);
#11029=ORIENTED_EDGE('',*,*,#8056,.T.);
#11030=ORIENTED_EDGE('',*,*,#8061,.T.);
#11031=ORIENTED_EDGE('',*,*,#8062,.F.);
#11032=ORIENTED_EDGE('',*,*,#8063,.T.);
#11033=ORIENTED_EDGE('',*,*,#8059,.T.);
#11034=ORIENTED_EDGE('',*,*,#8064,.T.);
#11035=ORIENTED_EDGE('',*,*,#8065,.F.);
#11036=ORIENTED_EDGE('',*,*,#8066,.T.);
#11037=ORIENTED_EDGE('',*,*,#8062,.T.);
#11038=ORIENTED_EDGE('',*,*,#8067,.T.);
#11039=ORIENTED_EDGE('',*,*,#8068,.F.);
#11040=ORIENTED_EDGE('',*,*,#8069,.T.);
#11041=ORIENTED_EDGE('',*,*,#8065,.T.);
#11042=ORIENTED_EDGE('',*,*,#8070,.T.);
#11043=ORIENTED_EDGE('',*,*,#8071,.F.);
#11044=ORIENTED_EDGE('',*,*,#8072,.T.);
#11045=ORIENTED_EDGE('',*,*,#8068,.T.);
#11046=ORIENTED_EDGE('',*,*,#8073,.T.);
#11047=ORIENTED_EDGE('',*,*,#8074,.F.);
#11048=ORIENTED_EDGE('',*,*,#8075,.T.);
#11049=ORIENTED_EDGE('',*,*,#8071,.T.);
#11050=ORIENTED_EDGE('',*,*,#8076,.T.);
#11051=ORIENTED_EDGE('',*,*,#8077,.F.);
#11052=ORIENTED_EDGE('',*,*,#8078,.T.);
#11053=ORIENTED_EDGE('',*,*,#8074,.T.);
#11054=ORIENTED_EDGE('',*,*,#8079,.T.);
#11055=ORIENTED_EDGE('',*,*,#8080,.F.);
#11056=ORIENTED_EDGE('',*,*,#8081,.T.);
#11057=ORIENTED_EDGE('',*,*,#8077,.T.);
#11058=ORIENTED_EDGE('',*,*,#8082,.T.);
#11059=ORIENTED_EDGE('',*,*,#8083,.F.);
#11060=ORIENTED_EDGE('',*,*,#8084,.T.);
#11061=ORIENTED_EDGE('',*,*,#8080,.T.);
#11062=ORIENTED_EDGE('',*,*,#8085,.T.);
#11063=ORIENTED_EDGE('',*,*,#8086,.F.);
#11064=ORIENTED_EDGE('',*,*,#8087,.T.);
#11065=ORIENTED_EDGE('',*,*,#8083,.T.);
#11066=ORIENTED_EDGE('',*,*,#8088,.T.);
#11067=ORIENTED_EDGE('',*,*,#8089,.F.);
#11068=ORIENTED_EDGE('',*,*,#8090,.T.);
#11069=ORIENTED_EDGE('',*,*,#8086,.T.);
#11070=ORIENTED_EDGE('',*,*,#8091,.T.);
#11071=ORIENTED_EDGE('',*,*,#8092,.F.);
#11072=ORIENTED_EDGE('',*,*,#8093,.T.);
#11073=ORIENTED_EDGE('',*,*,#8089,.T.);
#11074=ORIENTED_EDGE('',*,*,#8094,.T.);
#11075=ORIENTED_EDGE('',*,*,#8095,.F.);
#11076=ORIENTED_EDGE('',*,*,#8096,.T.);
#11077=ORIENTED_EDGE('',*,*,#8092,.T.);
#11078=ORIENTED_EDGE('',*,*,#8097,.T.);
#11079=ORIENTED_EDGE('',*,*,#8098,.F.);
#11080=ORIENTED_EDGE('',*,*,#8099,.T.);
#11081=ORIENTED_EDGE('',*,*,#8095,.T.);
#11082=ORIENTED_EDGE('',*,*,#8100,.T.);
#11083=ORIENTED_EDGE('',*,*,#8101,.F.);
#11084=ORIENTED_EDGE('',*,*,#8102,.T.);
#11085=ORIENTED_EDGE('',*,*,#8098,.T.);
#11086=ORIENTED_EDGE('',*,*,#8103,.T.);
#11087=ORIENTED_EDGE('',*,*,#8104,.F.);
#11088=ORIENTED_EDGE('',*,*,#8105,.T.);
#11089=ORIENTED_EDGE('',*,*,#8101,.T.);
#11090=ORIENTED_EDGE('',*,*,#8106,.T.);
#11091=ORIENTED_EDGE('',*,*,#8107,.F.);
#11092=ORIENTED_EDGE('',*,*,#8108,.T.);
#11093=ORIENTED_EDGE('',*,*,#8104,.T.);
#11094=ORIENTED_EDGE('',*,*,#8109,.T.);
#11095=ORIENTED_EDGE('',*,*,#8110,.F.);
#11096=ORIENTED_EDGE('',*,*,#8111,.T.);
#11097=ORIENTED_EDGE('',*,*,#8107,.T.);
#11098=ORIENTED_EDGE('',*,*,#8112,.T.);
#11099=ORIENTED_EDGE('',*,*,#8113,.F.);
#11100=ORIENTED_EDGE('',*,*,#8114,.T.);
#11101=ORIENTED_EDGE('',*,*,#8115,.F.);
#11102=ORIENTED_EDGE('',*,*,#8116,.F.);
#11103=ORIENTED_EDGE('',*,*,#8117,.T.);
#11104=ORIENTED_EDGE('',*,*,#8113,.T.);
#11105=ORIENTED_EDGE('',*,*,#8118,.F.);
#11106=ORIENTED_EDGE('',*,*,#8119,.F.);
#11107=ORIENTED_EDGE('',*,*,#8120,.F.);
#11108=ORIENTED_EDGE('',*,*,#8121,.T.);
#11109=ORIENTED_EDGE('',*,*,#8116,.T.);
#11110=ORIENTED_EDGE('',*,*,#8122,.F.);
#11111=ORIENTED_EDGE('',*,*,#8123,.F.);
#11112=ORIENTED_EDGE('',*,*,#8124,.T.);
#11113=ORIENTED_EDGE('',*,*,#8120,.T.);
#11114=ORIENTED_EDGE('',*,*,#8125,.F.);
#11115=ORIENTED_EDGE('',*,*,#8126,.F.);
#11116=ORIENTED_EDGE('',*,*,#8127,.T.);
#11117=ORIENTED_EDGE('',*,*,#8123,.T.);
#11118=ORIENTED_EDGE('',*,*,#8128,.F.);
#11119=ORIENTED_EDGE('',*,*,#8129,.F.);
#11120=ORIENTED_EDGE('',*,*,#8130,.T.);
#11121=ORIENTED_EDGE('',*,*,#8126,.T.);
#11122=ORIENTED_EDGE('',*,*,#8131,.F.);
#11123=ORIENTED_EDGE('',*,*,#8132,.F.);
#11124=ORIENTED_EDGE('',*,*,#8133,.T.);
#11125=ORIENTED_EDGE('',*,*,#8129,.T.);
#11126=ORIENTED_EDGE('',*,*,#8134,.F.);
#11127=ORIENTED_EDGE('',*,*,#8135,.F.);
#11128=ORIENTED_EDGE('',*,*,#8136,.T.);
#11129=ORIENTED_EDGE('',*,*,#8132,.T.);
#11130=ORIENTED_EDGE('',*,*,#8137,.F.);
#11131=ORIENTED_EDGE('',*,*,#8138,.F.);
#11132=ORIENTED_EDGE('',*,*,#8139,.T.);
#11133=ORIENTED_EDGE('',*,*,#8135,.T.);
#11134=ORIENTED_EDGE('',*,*,#8140,.F.);
#11135=ORIENTED_EDGE('',*,*,#8141,.F.);
#11136=ORIENTED_EDGE('',*,*,#8142,.T.);
#11137=ORIENTED_EDGE('',*,*,#8138,.T.);
#11138=ORIENTED_EDGE('',*,*,#8143,.F.);
#11139=ORIENTED_EDGE('',*,*,#8144,.F.);
#11140=ORIENTED_EDGE('',*,*,#8145,.T.);
#11141=ORIENTED_EDGE('',*,*,#8141,.T.);
#11142=ORIENTED_EDGE('',*,*,#8146,.F.);
#11143=ORIENTED_EDGE('',*,*,#8147,.F.);
#11144=ORIENTED_EDGE('',*,*,#8148,.T.);
#11145=ORIENTED_EDGE('',*,*,#8144,.T.);
#11146=ORIENTED_EDGE('',*,*,#8149,.F.);
#11147=ORIENTED_EDGE('',*,*,#8150,.F.);
#11148=ORIENTED_EDGE('',*,*,#8151,.T.);
#11149=ORIENTED_EDGE('',*,*,#8147,.T.);
#11150=ORIENTED_EDGE('',*,*,#8152,.F.);
#11151=ORIENTED_EDGE('',*,*,#8153,.F.);
#11152=ORIENTED_EDGE('',*,*,#8154,.T.);
#11153=ORIENTED_EDGE('',*,*,#8150,.T.);
#11154=ORIENTED_EDGE('',*,*,#8155,.F.);
#11155=ORIENTED_EDGE('',*,*,#8156,.F.);
#11156=ORIENTED_EDGE('',*,*,#8157,.T.);
#11157=ORIENTED_EDGE('',*,*,#8153,.T.);
#11158=ORIENTED_EDGE('',*,*,#8158,.F.);
#11159=ORIENTED_EDGE('',*,*,#8159,.F.);
#11160=ORIENTED_EDGE('',*,*,#8160,.T.);
#11161=ORIENTED_EDGE('',*,*,#8156,.T.);
#11162=ORIENTED_EDGE('',*,*,#8161,.F.);
#11163=ORIENTED_EDGE('',*,*,#8162,.F.);
#11164=ORIENTED_EDGE('',*,*,#8163,.T.);
#11165=ORIENTED_EDGE('',*,*,#8159,.T.);
#11166=ORIENTED_EDGE('',*,*,#8164,.F.);
#11167=ORIENTED_EDGE('',*,*,#8165,.F.);
#11168=ORIENTED_EDGE('',*,*,#8166,.T.);
#11169=ORIENTED_EDGE('',*,*,#8162,.T.);
#11170=ORIENTED_EDGE('',*,*,#8167,.F.);
#11171=ORIENTED_EDGE('',*,*,#8168,.F.);
#11172=ORIENTED_EDGE('',*,*,#8169,.T.);
#11173=ORIENTED_EDGE('',*,*,#8165,.T.);
#11174=ORIENTED_EDGE('',*,*,#8170,.F.);
#11175=ORIENTED_EDGE('',*,*,#8171,.F.);
#11176=ORIENTED_EDGE('',*,*,#8172,.T.);
#11177=ORIENTED_EDGE('',*,*,#8168,.T.);
#11178=ORIENTED_EDGE('',*,*,#8173,.F.);
#11179=ORIENTED_EDGE('',*,*,#8174,.F.);
#11180=ORIENTED_EDGE('',*,*,#8175,.T.);
#11181=ORIENTED_EDGE('',*,*,#8171,.T.);
#11182=ORIENTED_EDGE('',*,*,#8176,.F.);
#11183=ORIENTED_EDGE('',*,*,#8177,.F.);
#11184=ORIENTED_EDGE('',*,*,#8178,.T.);
#11185=ORIENTED_EDGE('',*,*,#8174,.T.);
#11186=ORIENTED_EDGE('',*,*,#8179,.F.);
#11187=ORIENTED_EDGE('',*,*,#8180,.F.);
#11188=ORIENTED_EDGE('',*,*,#8181,.T.);
#11189=ORIENTED_EDGE('',*,*,#8177,.T.);
#11190=ORIENTED_EDGE('',*,*,#8182,.F.);
#11191=ORIENTED_EDGE('',*,*,#8183,.F.);
#11192=ORIENTED_EDGE('',*,*,#8184,.T.);
#11193=ORIENTED_EDGE('',*,*,#8180,.T.);
#11194=ORIENTED_EDGE('',*,*,#8185,.F.);
#11195=ORIENTED_EDGE('',*,*,#8186,.F.);
#11196=ORIENTED_EDGE('',*,*,#8187,.T.);
#11197=ORIENTED_EDGE('',*,*,#8183,.T.);
#11198=ORIENTED_EDGE('',*,*,#8188,.F.);
#11199=ORIENTED_EDGE('',*,*,#8189,.F.);
#11200=ORIENTED_EDGE('',*,*,#8190,.T.);
#11201=ORIENTED_EDGE('',*,*,#8186,.T.);
#11202=ORIENTED_EDGE('',*,*,#8191,.F.);
#11203=ORIENTED_EDGE('',*,*,#8192,.F.);
#11204=ORIENTED_EDGE('',*,*,#8193,.T.);
#11205=ORIENTED_EDGE('',*,*,#8189,.T.);
#11206=ORIENTED_EDGE('',*,*,#8194,.F.);
#11207=ORIENTED_EDGE('',*,*,#8195,.F.);
#11208=ORIENTED_EDGE('',*,*,#8196,.T.);
#11209=ORIENTED_EDGE('',*,*,#8192,.T.);
#11210=ORIENTED_EDGE('',*,*,#8197,.F.);
#11211=ORIENTED_EDGE('',*,*,#8198,.F.);
#11212=ORIENTED_EDGE('',*,*,#8199,.T.);
#11213=ORIENTED_EDGE('',*,*,#8195,.T.);
#11214=ORIENTED_EDGE('',*,*,#8200,.F.);
#11215=ORIENTED_EDGE('',*,*,#8201,.F.);
#11216=ORIENTED_EDGE('',*,*,#8202,.T.);
#11217=ORIENTED_EDGE('',*,*,#8198,.T.);
#11218=ORIENTED_EDGE('',*,*,#8203,.F.);
#11219=ORIENTED_EDGE('',*,*,#8204,.F.);
#11220=ORIENTED_EDGE('',*,*,#8205,.T.);
#11221=ORIENTED_EDGE('',*,*,#8201,.T.);
#11222=ORIENTED_EDGE('',*,*,#8206,.F.);
#11223=ORIENTED_EDGE('',*,*,#8207,.F.);
#11224=ORIENTED_EDGE('',*,*,#8208,.T.);
#11225=ORIENTED_EDGE('',*,*,#8204,.T.);
#11226=ORIENTED_EDGE('',*,*,#8209,.F.);
#11227=ORIENTED_EDGE('',*,*,#8210,.F.);
#11228=ORIENTED_EDGE('',*,*,#8211,.T.);
#11229=ORIENTED_EDGE('',*,*,#8207,.T.);
#11230=ORIENTED_EDGE('',*,*,#8212,.F.);
#11231=ORIENTED_EDGE('',*,*,#8213,.F.);
#11232=ORIENTED_EDGE('',*,*,#8214,.T.);
#11233=ORIENTED_EDGE('',*,*,#8210,.T.);
#11234=ORIENTED_EDGE('',*,*,#8215,.F.);
#11235=ORIENTED_EDGE('',*,*,#8216,.F.);
#11236=ORIENTED_EDGE('',*,*,#8217,.T.);
#11237=ORIENTED_EDGE('',*,*,#8213,.T.);
#11238=ORIENTED_EDGE('',*,*,#8218,.F.);
#11239=ORIENTED_EDGE('',*,*,#8219,.F.);
#11240=ORIENTED_EDGE('',*,*,#8220,.T.);
#11241=ORIENTED_EDGE('',*,*,#8216,.T.);
#11242=ORIENTED_EDGE('',*,*,#8221,.F.);
#11243=ORIENTED_EDGE('',*,*,#8222,.F.);
#11244=ORIENTED_EDGE('',*,*,#8223,.T.);
#11245=ORIENTED_EDGE('',*,*,#8219,.T.);
#11246=ORIENTED_EDGE('',*,*,#8224,.F.);
#11247=ORIENTED_EDGE('',*,*,#8225,.F.);
#11248=ORIENTED_EDGE('',*,*,#8226,.T.);
#11249=ORIENTED_EDGE('',*,*,#8222,.T.);
#11250=ORIENTED_EDGE('',*,*,#8227,.F.);
#11251=ORIENTED_EDGE('',*,*,#8228,.F.);
#11252=ORIENTED_EDGE('',*,*,#8229,.T.);
#11253=ORIENTED_EDGE('',*,*,#8225,.T.);
#11254=ORIENTED_EDGE('',*,*,#8230,.F.);
#11255=ORIENTED_EDGE('',*,*,#8231,.F.);
#11256=ORIENTED_EDGE('',*,*,#8232,.T.);
#11257=ORIENTED_EDGE('',*,*,#8228,.T.);
#11258=ORIENTED_EDGE('',*,*,#8233,.F.);
#11259=ORIENTED_EDGE('',*,*,#8234,.F.);
#11260=ORIENTED_EDGE('',*,*,#8235,.T.);
#11261=ORIENTED_EDGE('',*,*,#8231,.T.);
#11262=ORIENTED_EDGE('',*,*,#8236,.F.);
#11263=ORIENTED_EDGE('',*,*,#8237,.F.);
#11264=ORIENTED_EDGE('',*,*,#8238,.T.);
#11265=ORIENTED_EDGE('',*,*,#8234,.T.);
#11266=ORIENTED_EDGE('',*,*,#8239,.F.);
#11267=ORIENTED_EDGE('',*,*,#8240,.F.);
#11268=ORIENTED_EDGE('',*,*,#8241,.T.);
#11269=ORIENTED_EDGE('',*,*,#8237,.T.);
#11270=ORIENTED_EDGE('',*,*,#8242,.F.);
#11271=ORIENTED_EDGE('',*,*,#8243,.F.);
#11272=ORIENTED_EDGE('',*,*,#8244,.T.);
#11273=ORIENTED_EDGE('',*,*,#8240,.T.);
#11274=ORIENTED_EDGE('',*,*,#8245,.F.);
#11275=ORIENTED_EDGE('',*,*,#8246,.F.);
#11276=ORIENTED_EDGE('',*,*,#8247,.T.);
#11277=ORIENTED_EDGE('',*,*,#8243,.T.);
#11278=ORIENTED_EDGE('',*,*,#8248,.F.);
#11279=ORIENTED_EDGE('',*,*,#8249,.F.);
#11280=ORIENTED_EDGE('',*,*,#8250,.T.);
#11281=ORIENTED_EDGE('',*,*,#8246,.T.);
#11282=ORIENTED_EDGE('',*,*,#8251,.F.);
#11283=ORIENTED_EDGE('',*,*,#8252,.F.);
#11284=ORIENTED_EDGE('',*,*,#8253,.T.);
#11285=ORIENTED_EDGE('',*,*,#8249,.T.);
#11286=ORIENTED_EDGE('',*,*,#8254,.F.);
#11287=ORIENTED_EDGE('',*,*,#8255,.F.);
#11288=ORIENTED_EDGE('',*,*,#8256,.T.);
#11289=ORIENTED_EDGE('',*,*,#8252,.T.);
#11290=ORIENTED_EDGE('',*,*,#8257,.F.);
#11291=ORIENTED_EDGE('',*,*,#8258,.F.);
#11292=ORIENTED_EDGE('',*,*,#8259,.T.);
#11293=ORIENTED_EDGE('',*,*,#8255,.T.);
#11294=ORIENTED_EDGE('',*,*,#8260,.F.);
#11295=ORIENTED_EDGE('',*,*,#8261,.F.);
#11296=ORIENTED_EDGE('',*,*,#8262,.T.);
#11297=ORIENTED_EDGE('',*,*,#8258,.T.);
#11298=ORIENTED_EDGE('',*,*,#8263,.F.);
#11299=ORIENTED_EDGE('',*,*,#8264,.F.);
#11300=ORIENTED_EDGE('',*,*,#8265,.T.);
#11301=ORIENTED_EDGE('',*,*,#8261,.T.);
#11302=ORIENTED_EDGE('',*,*,#8266,.F.);
#11303=ORIENTED_EDGE('',*,*,#8267,.F.);
#11304=ORIENTED_EDGE('',*,*,#8268,.T.);
#11305=ORIENTED_EDGE('',*,*,#8264,.T.);
#11306=ORIENTED_EDGE('',*,*,#8269,.F.);
#11307=ORIENTED_EDGE('',*,*,#8270,.F.);
#11308=ORIENTED_EDGE('',*,*,#8271,.T.);
#11309=ORIENTED_EDGE('',*,*,#8267,.T.);
#11310=ORIENTED_EDGE('',*,*,#8272,.F.);
#11311=ORIENTED_EDGE('',*,*,#8273,.F.);
#11312=ORIENTED_EDGE('',*,*,#8274,.T.);
#11313=ORIENTED_EDGE('',*,*,#8270,.T.);
#11314=ORIENTED_EDGE('',*,*,#8275,.F.);
#11315=ORIENTED_EDGE('',*,*,#8276,.F.);
#11316=ORIENTED_EDGE('',*,*,#8277,.T.);
#11317=ORIENTED_EDGE('',*,*,#8273,.T.);
#11318=ORIENTED_EDGE('',*,*,#8278,.F.);
#11319=ORIENTED_EDGE('',*,*,#8279,.F.);
#11320=ORIENTED_EDGE('',*,*,#8280,.T.);
#11321=ORIENTED_EDGE('',*,*,#8276,.T.);
#11322=ORIENTED_EDGE('',*,*,#8281,.F.);
#11323=ORIENTED_EDGE('',*,*,#8282,.F.);
#11324=ORIENTED_EDGE('',*,*,#8283,.T.);
#11325=ORIENTED_EDGE('',*,*,#8279,.T.);
#11326=ORIENTED_EDGE('',*,*,#8284,.F.);
#11327=ORIENTED_EDGE('',*,*,#8285,.F.);
#11328=ORIENTED_EDGE('',*,*,#8286,.T.);
#11329=ORIENTED_EDGE('',*,*,#8282,.T.);
#11330=ORIENTED_EDGE('',*,*,#8287,.F.);
#11331=ORIENTED_EDGE('',*,*,#8288,.F.);
#11332=ORIENTED_EDGE('',*,*,#8289,.T.);
#11333=ORIENTED_EDGE('',*,*,#8285,.T.);
#11334=ORIENTED_EDGE('',*,*,#8290,.F.);
#11335=ORIENTED_EDGE('',*,*,#8291,.F.);
#11336=ORIENTED_EDGE('',*,*,#8292,.T.);
#11337=ORIENTED_EDGE('',*,*,#8288,.T.);
#11338=ORIENTED_EDGE('',*,*,#8293,.F.);
#11339=ORIENTED_EDGE('',*,*,#8294,.F.);
#11340=ORIENTED_EDGE('',*,*,#8295,.T.);
#11341=ORIENTED_EDGE('',*,*,#8291,.T.);
#11342=ORIENTED_EDGE('',*,*,#8296,.F.);
#11343=ORIENTED_EDGE('',*,*,#8297,.F.);
#11344=ORIENTED_EDGE('',*,*,#8298,.T.);
#11345=ORIENTED_EDGE('',*,*,#8294,.T.);
#11346=ORIENTED_EDGE('',*,*,#8299,.F.);
#11347=ORIENTED_EDGE('',*,*,#8300,.F.);
#11348=ORIENTED_EDGE('',*,*,#8301,.T.);
#11349=ORIENTED_EDGE('',*,*,#8297,.T.);
#11350=ORIENTED_EDGE('',*,*,#8302,.F.);
#11351=ORIENTED_EDGE('',*,*,#8303,.T.);
#11352=ORIENTED_EDGE('',*,*,#8304,.T.);
#11353=ORIENTED_EDGE('',*,*,#7925,.F.);
#11354=ORIENTED_EDGE('',*,*,#8305,.T.);
#11355=ORIENTED_EDGE('',*,*,#8306,.T.);
#11356=ORIENTED_EDGE('',*,*,#8303,.F.);
#11357=ORIENTED_EDGE('',*,*,#8307,.T.);
#11358=ORIENTED_EDGE('',*,*,#8308,.T.);
#11359=ORIENTED_EDGE('',*,*,#8307,.F.);
#11360=ORIENTED_EDGE('',*,*,#8308,.F.);
#11361=ORIENTED_EDGE('',*,*,#8309,.F.);
#11362=ORIENTED_EDGE('',*,*,#8310,.F.);
#11363=ORIENTED_EDGE('',*,*,#8112,.F.);
#11364=ORIENTED_EDGE('',*,*,#8109,.F.);
#11365=ORIENTED_EDGE('',*,*,#8106,.F.);
#11366=ORIENTED_EDGE('',*,*,#8103,.F.);
#11367=ORIENTED_EDGE('',*,*,#8100,.F.);
#11368=ORIENTED_EDGE('',*,*,#8097,.F.);
#11369=ORIENTED_EDGE('',*,*,#8094,.F.);
#11370=ORIENTED_EDGE('',*,*,#8091,.F.);
#11371=ORIENTED_EDGE('',*,*,#8088,.F.);
#11372=ORIENTED_EDGE('',*,*,#8085,.F.);
#11373=ORIENTED_EDGE('',*,*,#8082,.F.);
#11374=ORIENTED_EDGE('',*,*,#8079,.F.);
#11375=ORIENTED_EDGE('',*,*,#8076,.F.);
#11376=ORIENTED_EDGE('',*,*,#8073,.F.);
#11377=ORIENTED_EDGE('',*,*,#8070,.F.);
#11378=ORIENTED_EDGE('',*,*,#8067,.F.);
#11379=ORIENTED_EDGE('',*,*,#8064,.F.);
#11380=ORIENTED_EDGE('',*,*,#8061,.F.);
#11381=ORIENTED_EDGE('',*,*,#8058,.F.);
#11382=ORIENTED_EDGE('',*,*,#8055,.F.);
#11383=ORIENTED_EDGE('',*,*,#8052,.F.);
#11384=ORIENTED_EDGE('',*,*,#8049,.F.);
#11385=ORIENTED_EDGE('',*,*,#8046,.F.);
#11386=ORIENTED_EDGE('',*,*,#8043,.F.);
#11387=ORIENTED_EDGE('',*,*,#8040,.F.);
#11388=ORIENTED_EDGE('',*,*,#8037,.F.);
#11389=ORIENTED_EDGE('',*,*,#8034,.F.);
#11390=ORIENTED_EDGE('',*,*,#8031,.F.);
#11391=ORIENTED_EDGE('',*,*,#8028,.F.);
#11392=ORIENTED_EDGE('',*,*,#8025,.F.);
#11393=ORIENTED_EDGE('',*,*,#8022,.F.);
#11394=ORIENTED_EDGE('',*,*,#8019,.F.);
#11395=ORIENTED_EDGE('',*,*,#8016,.F.);
#11396=ORIENTED_EDGE('',*,*,#8013,.F.);
#11397=ORIENTED_EDGE('',*,*,#8010,.F.);
#11398=ORIENTED_EDGE('',*,*,#8007,.F.);
#11399=ORIENTED_EDGE('',*,*,#8004,.F.);
#11400=ORIENTED_EDGE('',*,*,#8001,.F.);
#11401=ORIENTED_EDGE('',*,*,#7998,.F.);
#11402=ORIENTED_EDGE('',*,*,#7995,.F.);
#11403=ORIENTED_EDGE('',*,*,#7992,.F.);
#11404=ORIENTED_EDGE('',*,*,#7989,.F.);
#11405=ORIENTED_EDGE('',*,*,#7986,.F.);
#11406=ORIENTED_EDGE('',*,*,#7983,.F.);
#11407=ORIENTED_EDGE('',*,*,#7980,.F.);
#11408=ORIENTED_EDGE('',*,*,#7977,.F.);
#11409=ORIENTED_EDGE('',*,*,#7974,.F.);
#11410=ORIENTED_EDGE('',*,*,#7971,.F.);
#11411=ORIENTED_EDGE('',*,*,#7968,.F.);
#11412=ORIENTED_EDGE('',*,*,#7965,.F.);
#11413=ORIENTED_EDGE('',*,*,#7962,.F.);
#11414=ORIENTED_EDGE('',*,*,#7959,.F.);
#11415=ORIENTED_EDGE('',*,*,#7956,.F.);
#11416=ORIENTED_EDGE('',*,*,#7953,.F.);
#11417=ORIENTED_EDGE('',*,*,#7950,.F.);
#11418=ORIENTED_EDGE('',*,*,#7947,.F.);
#11419=ORIENTED_EDGE('',*,*,#7944,.F.);
#11420=ORIENTED_EDGE('',*,*,#7941,.F.);
#11421=ORIENTED_EDGE('',*,*,#7938,.F.);
#11422=ORIENTED_EDGE('',*,*,#7935,.F.);
#11423=ORIENTED_EDGE('',*,*,#7932,.F.);
#11424=ORIENTED_EDGE('',*,*,#7929,.F.);
#11425=ORIENTED_EDGE('',*,*,#7926,.F.);
#11426=ORIENTED_EDGE('',*,*,#8304,.F.);
#11427=ORIENTED_EDGE('',*,*,#8311,.T.);
#11428=ORIENTED_EDGE('',*,*,#8302,.T.);
#11429=ORIENTED_EDGE('',*,*,#8299,.T.);
#11430=ORIENTED_EDGE('',*,*,#8296,.T.);
#11431=ORIENTED_EDGE('',*,*,#8293,.T.);
#11432=ORIENTED_EDGE('',*,*,#8290,.T.);
#11433=ORIENTED_EDGE('',*,*,#8287,.T.);
#11434=ORIENTED_EDGE('',*,*,#8284,.T.);
#11435=ORIENTED_EDGE('',*,*,#8281,.T.);
#11436=ORIENTED_EDGE('',*,*,#8278,.T.);
#11437=ORIENTED_EDGE('',*,*,#8275,.T.);
#11438=ORIENTED_EDGE('',*,*,#8272,.T.);
#11439=ORIENTED_EDGE('',*,*,#8269,.T.);
#11440=ORIENTED_EDGE('',*,*,#8266,.T.);
#11441=ORIENTED_EDGE('',*,*,#8263,.T.);
#11442=ORIENTED_EDGE('',*,*,#8260,.T.);
#11443=ORIENTED_EDGE('',*,*,#8257,.T.);
#11444=ORIENTED_EDGE('',*,*,#8254,.T.);
#11445=ORIENTED_EDGE('',*,*,#8251,.T.);
#11446=ORIENTED_EDGE('',*,*,#8248,.T.);
#11447=ORIENTED_EDGE('',*,*,#8245,.T.);
#11448=ORIENTED_EDGE('',*,*,#8242,.T.);
#11449=ORIENTED_EDGE('',*,*,#8239,.T.);
#11450=ORIENTED_EDGE('',*,*,#8236,.T.);
#11451=ORIENTED_EDGE('',*,*,#8233,.T.);
#11452=ORIENTED_EDGE('',*,*,#8230,.T.);
#11453=ORIENTED_EDGE('',*,*,#8227,.T.);
#11454=ORIENTED_EDGE('',*,*,#8224,.T.);
#11455=ORIENTED_EDGE('',*,*,#8221,.T.);
#11456=ORIENTED_EDGE('',*,*,#8218,.T.);
#11457=ORIENTED_EDGE('',*,*,#8215,.T.);
#11458=ORIENTED_EDGE('',*,*,#8212,.T.);
#11459=ORIENTED_EDGE('',*,*,#8209,.T.);
#11460=ORIENTED_EDGE('',*,*,#8206,.T.);
#11461=ORIENTED_EDGE('',*,*,#8203,.T.);
#11462=ORIENTED_EDGE('',*,*,#8200,.T.);
#11463=ORIENTED_EDGE('',*,*,#8197,.T.);
#11464=ORIENTED_EDGE('',*,*,#8194,.T.);
#11465=ORIENTED_EDGE('',*,*,#8191,.T.);
#11466=ORIENTED_EDGE('',*,*,#8188,.T.);
#11467=ORIENTED_EDGE('',*,*,#8185,.T.);
#11468=ORIENTED_EDGE('',*,*,#8182,.T.);
#11469=ORIENTED_EDGE('',*,*,#8179,.T.);
#11470=ORIENTED_EDGE('',*,*,#8176,.T.);
#11471=ORIENTED_EDGE('',*,*,#8173,.T.);
#11472=ORIENTED_EDGE('',*,*,#8170,.T.);
#11473=ORIENTED_EDGE('',*,*,#8167,.T.);
#11474=ORIENTED_EDGE('',*,*,#8164,.T.);
#11475=ORIENTED_EDGE('',*,*,#8161,.T.);
#11476=ORIENTED_EDGE('',*,*,#8158,.T.);
#11477=ORIENTED_EDGE('',*,*,#8155,.T.);
#11478=ORIENTED_EDGE('',*,*,#8152,.T.);
#11479=ORIENTED_EDGE('',*,*,#8149,.T.);
#11480=ORIENTED_EDGE('',*,*,#8146,.T.);
#11481=ORIENTED_EDGE('',*,*,#8143,.T.);
#11482=ORIENTED_EDGE('',*,*,#8140,.T.);
#11483=ORIENTED_EDGE('',*,*,#8137,.T.);
#11484=ORIENTED_EDGE('',*,*,#8134,.T.);
#11485=ORIENTED_EDGE('',*,*,#8131,.T.);
#11486=ORIENTED_EDGE('',*,*,#8128,.T.);
#11487=ORIENTED_EDGE('',*,*,#8125,.T.);
#11488=ORIENTED_EDGE('',*,*,#8122,.T.);
#11489=ORIENTED_EDGE('',*,*,#8119,.T.);
#11490=ORIENTED_EDGE('',*,*,#8300,.T.);
#11491=ORIENTED_EDGE('',*,*,#8311,.F.);
#11492=ORIENTED_EDGE('',*,*,#8306,.F.);
#11493=ORIENTED_EDGE('',*,*,#8312,.T.);
#11494=ORIENTED_EDGE('',*,*,#8313,.F.);
#11495=ORIENTED_EDGE('',*,*,#8114,.F.);
#11496=ORIENTED_EDGE('',*,*,#8117,.F.);
#11497=ORIENTED_EDGE('',*,*,#8121,.F.);
#11498=ORIENTED_EDGE('',*,*,#8124,.F.);
#11499=ORIENTED_EDGE('',*,*,#8127,.F.);
#11500=ORIENTED_EDGE('',*,*,#8130,.F.);
#11501=ORIENTED_EDGE('',*,*,#8133,.F.);
#11502=ORIENTED_EDGE('',*,*,#8136,.F.);
#11503=ORIENTED_EDGE('',*,*,#8139,.F.);
#11504=ORIENTED_EDGE('',*,*,#8142,.F.);
#11505=ORIENTED_EDGE('',*,*,#8145,.F.);
#11506=ORIENTED_EDGE('',*,*,#8148,.F.);
#11507=ORIENTED_EDGE('',*,*,#8151,.F.);
#11508=ORIENTED_EDGE('',*,*,#8154,.F.);
#11509=ORIENTED_EDGE('',*,*,#8157,.F.);
#11510=ORIENTED_EDGE('',*,*,#8160,.F.);
#11511=ORIENTED_EDGE('',*,*,#8163,.F.);
#11512=ORIENTED_EDGE('',*,*,#8166,.F.);
#11513=ORIENTED_EDGE('',*,*,#8169,.F.);
#11514=ORIENTED_EDGE('',*,*,#8172,.F.);
#11515=ORIENTED_EDGE('',*,*,#8175,.F.);
#11516=ORIENTED_EDGE('',*,*,#8178,.F.);
#11517=ORIENTED_EDGE('',*,*,#8181,.F.);
#11518=ORIENTED_EDGE('',*,*,#8184,.F.);
#11519=ORIENTED_EDGE('',*,*,#8187,.F.);
#11520=ORIENTED_EDGE('',*,*,#8190,.F.);
#11521=ORIENTED_EDGE('',*,*,#8193,.F.);
#11522=ORIENTED_EDGE('',*,*,#8196,.F.);
#11523=ORIENTED_EDGE('',*,*,#8199,.F.);
#11524=ORIENTED_EDGE('',*,*,#8202,.F.);
#11525=ORIENTED_EDGE('',*,*,#8205,.F.);
#11526=ORIENTED_EDGE('',*,*,#8208,.F.);
#11527=ORIENTED_EDGE('',*,*,#8211,.F.);
#11528=ORIENTED_EDGE('',*,*,#8214,.F.);
#11529=ORIENTED_EDGE('',*,*,#8217,.F.);
#11530=ORIENTED_EDGE('',*,*,#8220,.F.);
#11531=ORIENTED_EDGE('',*,*,#8223,.F.);
#11532=ORIENTED_EDGE('',*,*,#8226,.F.);
#11533=ORIENTED_EDGE('',*,*,#8229,.F.);
#11534=ORIENTED_EDGE('',*,*,#8232,.F.);
#11535=ORIENTED_EDGE('',*,*,#8235,.F.);
#11536=ORIENTED_EDGE('',*,*,#8238,.F.);
#11537=ORIENTED_EDGE('',*,*,#8241,.F.);
#11538=ORIENTED_EDGE('',*,*,#8244,.F.);
#11539=ORIENTED_EDGE('',*,*,#8247,.F.);
#11540=ORIENTED_EDGE('',*,*,#8250,.F.);
#11541=ORIENTED_EDGE('',*,*,#8253,.F.);
#11542=ORIENTED_EDGE('',*,*,#8256,.F.);
#11543=ORIENTED_EDGE('',*,*,#8259,.F.);
#11544=ORIENTED_EDGE('',*,*,#8262,.F.);
#11545=ORIENTED_EDGE('',*,*,#8265,.F.);
#11546=ORIENTED_EDGE('',*,*,#8268,.F.);
#11547=ORIENTED_EDGE('',*,*,#8271,.F.);
#11548=ORIENTED_EDGE('',*,*,#8274,.F.);
#11549=ORIENTED_EDGE('',*,*,#8277,.F.);
#11550=ORIENTED_EDGE('',*,*,#8280,.F.);
#11551=ORIENTED_EDGE('',*,*,#8283,.F.);
#11552=ORIENTED_EDGE('',*,*,#8286,.F.);
#11553=ORIENTED_EDGE('',*,*,#8289,.F.);
#11554=ORIENTED_EDGE('',*,*,#8292,.F.);
#11555=ORIENTED_EDGE('',*,*,#8295,.F.);
#11556=ORIENTED_EDGE('',*,*,#8298,.F.);
#11557=ORIENTED_EDGE('',*,*,#8301,.F.);
#11558=ORIENTED_EDGE('',*,*,#8312,.F.);
#11559=ORIENTED_EDGE('',*,*,#8305,.F.);
#11560=ORIENTED_EDGE('',*,*,#7924,.F.);
#11561=ORIENTED_EDGE('',*,*,#7928,.F.);
#11562=ORIENTED_EDGE('',*,*,#7931,.F.);
#11563=ORIENTED_EDGE('',*,*,#7934,.F.);
#11564=ORIENTED_EDGE('',*,*,#7937,.F.);
#11565=ORIENTED_EDGE('',*,*,#7940,.F.);
#11566=ORIENTED_EDGE('',*,*,#7943,.F.);
#11567=ORIENTED_EDGE('',*,*,#7946,.F.);
#11568=ORIENTED_EDGE('',*,*,#7949,.F.);
#11569=ORIENTED_EDGE('',*,*,#7952,.F.);
#11570=ORIENTED_EDGE('',*,*,#7955,.F.);
#11571=ORIENTED_EDGE('',*,*,#7958,.F.);
#11572=ORIENTED_EDGE('',*,*,#7961,.F.);
#11573=ORIENTED_EDGE('',*,*,#7964,.F.);
#11574=ORIENTED_EDGE('',*,*,#7967,.F.);
#11575=ORIENTED_EDGE('',*,*,#7970,.F.);
#11576=ORIENTED_EDGE('',*,*,#7973,.F.);
#11577=ORIENTED_EDGE('',*,*,#7976,.F.);
#11578=ORIENTED_EDGE('',*,*,#7979,.F.);
#11579=ORIENTED_EDGE('',*,*,#7982,.F.);
#11580=ORIENTED_EDGE('',*,*,#7985,.F.);
#11581=ORIENTED_EDGE('',*,*,#7988,.F.);
#11582=ORIENTED_EDGE('',*,*,#7991,.F.);
#11583=ORIENTED_EDGE('',*,*,#7994,.F.);
#11584=ORIENTED_EDGE('',*,*,#7997,.F.);
#11585=ORIENTED_EDGE('',*,*,#8000,.F.);
#11586=ORIENTED_EDGE('',*,*,#8003,.F.);
#11587=ORIENTED_EDGE('',*,*,#8006,.F.);
#11588=ORIENTED_EDGE('',*,*,#8009,.F.);
#11589=ORIENTED_EDGE('',*,*,#8012,.F.);
#11590=ORIENTED_EDGE('',*,*,#8015,.F.);
#11591=ORIENTED_EDGE('',*,*,#8018,.F.);
#11592=ORIENTED_EDGE('',*,*,#8021,.F.);
#11593=ORIENTED_EDGE('',*,*,#8024,.F.);
#11594=ORIENTED_EDGE('',*,*,#8027,.F.);
#11595=ORIENTED_EDGE('',*,*,#8030,.F.);
#11596=ORIENTED_EDGE('',*,*,#8033,.F.);
#11597=ORIENTED_EDGE('',*,*,#8036,.F.);
#11598=ORIENTED_EDGE('',*,*,#8039,.F.);
#11599=ORIENTED_EDGE('',*,*,#8042,.F.);
#11600=ORIENTED_EDGE('',*,*,#8045,.F.);
#11601=ORIENTED_EDGE('',*,*,#8048,.F.);
#11602=ORIENTED_EDGE('',*,*,#8051,.F.);
#11603=ORIENTED_EDGE('',*,*,#8054,.F.);
#11604=ORIENTED_EDGE('',*,*,#8057,.F.);
#11605=ORIENTED_EDGE('',*,*,#8060,.F.);
#11606=ORIENTED_EDGE('',*,*,#8063,.F.);
#11607=ORIENTED_EDGE('',*,*,#8066,.F.);
#11608=ORIENTED_EDGE('',*,*,#8069,.F.);
#11609=ORIENTED_EDGE('',*,*,#8072,.F.);
#11610=ORIENTED_EDGE('',*,*,#8075,.F.);
#11611=ORIENTED_EDGE('',*,*,#8078,.F.);
#11612=ORIENTED_EDGE('',*,*,#8081,.F.);
#11613=ORIENTED_EDGE('',*,*,#8084,.F.);
#11614=ORIENTED_EDGE('',*,*,#8087,.F.);
#11615=ORIENTED_EDGE('',*,*,#8090,.F.);
#11616=ORIENTED_EDGE('',*,*,#8093,.F.);
#11617=ORIENTED_EDGE('',*,*,#8096,.F.);
#11618=ORIENTED_EDGE('',*,*,#8099,.F.);
#11619=ORIENTED_EDGE('',*,*,#8102,.F.);
#11620=ORIENTED_EDGE('',*,*,#8105,.F.);
#11621=ORIENTED_EDGE('',*,*,#8108,.F.);
#11622=ORIENTED_EDGE('',*,*,#8111,.F.);
#11623=ORIENTED_EDGE('',*,*,#8314,.F.);
#11624=ORIENTED_EDGE('',*,*,#8315,.F.);
#11625=ORIENTED_EDGE('',*,*,#8316,.T.);
#11626=ORIENTED_EDGE('',*,*,#8317,.F.);
#11627=ORIENTED_EDGE('',*,*,#8318,.F.);
#11628=ORIENTED_EDGE('',*,*,#8319,.F.);
#11629=ORIENTED_EDGE('',*,*,#8318,.T.);
#11630=ORIENTED_EDGE('',*,*,#8320,.T.);
#11631=ORIENTED_EDGE('',*,*,#8321,.T.);
#11632=ORIENTED_EDGE('',*,*,#8320,.F.);
#11633=ORIENTED_EDGE('',*,*,#8317,.T.);
#11634=ORIENTED_EDGE('',*,*,#8322,.T.);
#11635=ORIENTED_EDGE('',*,*,#8323,.F.);
#11636=ORIENTED_EDGE('',*,*,#8324,.F.);
#11637=ORIENTED_EDGE('',*,*,#8321,.F.);
#11638=ORIENTED_EDGE('',*,*,#8323,.T.);
#11639=ORIENTED_EDGE('',*,*,#8325,.T.);
#11640=ORIENTED_EDGE('',*,*,#8326,.F.);
#11641=ORIENTED_EDGE('',*,*,#8325,.F.);
#11642=ORIENTED_EDGE('',*,*,#8322,.F.);
#11643=ORIENTED_EDGE('',*,*,#8316,.F.);
#11644=ORIENTED_EDGE('',*,*,#8327,.F.);
#11645=ORIENTED_EDGE('',*,*,#8328,.T.);
#11646=ORIENTED_EDGE('',*,*,#8329,.F.);
#11647=ORIENTED_EDGE('',*,*,#8328,.F.);
#11648=ORIENTED_EDGE('',*,*,#8324,.T.);
#11649=ORIENTED_EDGE('',*,*,#8326,.T.);
#11650=ORIENTED_EDGE('',*,*,#8315,.T.);
#11651=ORIENTED_EDGE('',*,*,#8319,.T.);
#11652=ORIENTED_EDGE('',*,*,#8327,.T.);
#11653=ORIENTED_EDGE('',*,*,#8330,.F.);
#11654=ORIENTED_EDGE('',*,*,#8331,.T.);
#11655=ORIENTED_EDGE('',*,*,#8309,.T.);
#11656=ORIENTED_EDGE('',*,*,#8118,.T.);
#11657=ORIENTED_EDGE('',*,*,#8115,.T.);
#11658=ORIENTED_EDGE('',*,*,#8313,.T.);
#11659=ORIENTED_EDGE('',*,*,#8332,.F.);
#11660=ORIENTED_EDGE('',*,*,#8333,.T.);
#11661=ORIENTED_EDGE('',*,*,#8330,.T.);
#11662=ORIENTED_EDGE('',*,*,#8333,.F.);
#11663=ORIENTED_EDGE('',*,*,#8332,.T.);
#11664=ORIENTED_EDGE('',*,*,#8329,.T.);
#11665=ORIENTED_EDGE('',*,*,#8110,.T.);
#11666=ORIENTED_EDGE('',*,*,#8310,.T.);
#11667=ORIENTED_EDGE('',*,*,#8331,.F.);
#11668=ORIENTED_EDGE('',*,*,#8314,.T.);
#11669=ORIENTED_EDGE('',*,*,#8334,.F.);
#11670=ORIENTED_EDGE('',*,*,#8335,.T.);
#11671=ORIENTED_EDGE('',*,*,#8336,.T.);
#11672=ORIENTED_EDGE('',*,*,#8335,.F.);
#11673=ORIENTED_EDGE('',*,*,#8337,.F.);
#11674=ORIENTED_EDGE('',*,*,#8338,.T.);
#11675=ORIENTED_EDGE('',*,*,#8339,.T.);
#11676=ORIENTED_EDGE('',*,*,#8338,.F.);
#11677=ORIENTED_EDGE('',*,*,#8337,.T.);
#11678=ORIENTED_EDGE('',*,*,#8334,.T.);
#11679=ORIENTED_EDGE('',*,*,#8339,.F.);
#11680=ORIENTED_EDGE('',*,*,#8336,.F.);
#11681=ORIENTED_EDGE('',*,*,#8340,.F.);
#11682=ORIENTED_EDGE('',*,*,#8341,.T.);
#11683=ORIENTED_EDGE('',*,*,#8342,.F.);
#11684=ORIENTED_EDGE('',*,*,#8343,.F.);
#11685=ORIENTED_EDGE('',*,*,#8344,.F.);
#11686=ORIENTED_EDGE('',*,*,#8341,.F.);
#11687=ORIENTED_EDGE('',*,*,#8345,.F.);
#11688=ORIENTED_EDGE('',*,*,#8346,.T.);
#11689=ORIENTED_EDGE('',*,*,#8347,.F.);
#11690=ORIENTED_EDGE('',*,*,#8348,.F.);
#11691=ORIENTED_EDGE('',*,*,#8346,.F.);
#11692=ORIENTED_EDGE('',*,*,#8349,.F.);
#11693=ORIENTED_EDGE('',*,*,#8343,.T.);
#11694=ORIENTED_EDGE('',*,*,#8350,.F.);
#11695=ORIENTED_EDGE('',*,*,#8351,.T.);
#11696=ORIENTED_EDGE('',*,*,#8352,.T.);
#11697=ORIENTED_EDGE('',*,*,#8351,.F.);
#11698=ORIENTED_EDGE('',*,*,#8344,.T.);
#11699=ORIENTED_EDGE('',*,*,#8349,.T.);
#11700=ORIENTED_EDGE('',*,*,#8342,.T.);
#11701=ORIENTED_EDGE('',*,*,#8345,.T.);
#11702=ORIENTED_EDGE('',*,*,#8340,.T.);
#11703=ORIENTED_EDGE('',*,*,#8353,.F.);
#11704=ORIENTED_EDGE('',*,*,#8354,.T.);
#11705=ORIENTED_EDGE('',*,*,#8355,.T.);
#11706=ORIENTED_EDGE('',*,*,#8354,.F.);
#11707=ORIENTED_EDGE('',*,*,#8347,.T.);
#11708=ORIENTED_EDGE('',*,*,#8348,.T.);
#11709=ORIENTED_EDGE('',*,*,#8353,.T.);
#11710=ORIENTED_EDGE('',*,*,#8350,.T.);
#11711=ORIENTED_EDGE('',*,*,#8355,.F.);
#11712=ORIENTED_EDGE('',*,*,#8352,.F.);
#11713=ORIENTED_EDGE('',*,*,#8356,.F.);
#11714=ORIENTED_EDGE('',*,*,#8357,.T.);
#11715=ORIENTED_EDGE('',*,*,#8358,.F.);
#11716=ORIENTED_EDGE('',*,*,#8357,.F.);
#11717=ORIENTED_EDGE('',*,*,#8359,.F.);
#11718=ORIENTED_EDGE('',*,*,#8360,.T.);
#11719=ORIENTED_EDGE('',*,*,#8361,.F.);
#11720=ORIENTED_EDGE('',*,*,#8362,.F.);
#11721=ORIENTED_EDGE('',*,*,#8363,.F.);
#11722=ORIENTED_EDGE('',*,*,#8360,.F.);
#11723=ORIENTED_EDGE('',*,*,#8364,.F.);
#11724=ORIENTED_EDGE('',*,*,#8365,.T.);
#11725=ORIENTED_EDGE('',*,*,#8366,.F.);
#11726=ORIENTED_EDGE('',*,*,#8367,.F.);
#11727=ORIENTED_EDGE('',*,*,#8365,.F.);
#11728=ORIENTED_EDGE('',*,*,#8368,.F.);
#11729=ORIENTED_EDGE('',*,*,#8362,.T.);
#11730=ORIENTED_EDGE('',*,*,#8369,.F.);
#11731=ORIENTED_EDGE('',*,*,#8370,.F.);
#11732=ORIENTED_EDGE('',*,*,#8371,.F.);
#11733=ORIENTED_EDGE('',*,*,#8372,.F.);
#11734=ORIENTED_EDGE('',*,*,#8373,.F.);
#11735=ORIENTED_EDGE('',*,*,#8374,.F.);
#11736=ORIENTED_EDGE('',*,*,#8375,.F.);
#11737=ORIENTED_EDGE('',*,*,#8376,.F.);
#11738=ORIENTED_EDGE('',*,*,#8377,.F.);
#11739=ORIENTED_EDGE('',*,*,#8370,.T.);
#11740=ORIENTED_EDGE('',*,*,#8378,.F.);
#11741=ORIENTED_EDGE('',*,*,#8379,.F.);
#11742=ORIENTED_EDGE('',*,*,#8380,.F.);
#11743=ORIENTED_EDGE('',*,*,#8381,.F.);
#11744=ORIENTED_EDGE('',*,*,#8382,.F.);
#11745=ORIENTED_EDGE('',*,*,#8376,.T.);
#11746=ORIENTED_EDGE('',*,*,#8383,.T.);
#11747=ORIENTED_EDGE('',*,*,#8358,.T.);
#11748=ORIENTED_EDGE('',*,*,#8378,.T.);
#11749=ORIENTED_EDGE('',*,*,#8375,.T.);
#11750=ORIENTED_EDGE('',*,*,#8369,.T.);
#11751=ORIENTED_EDGE('',*,*,#8384,.T.);
#11752=ORIENTED_EDGE('',*,*,#8385,.F.);
#11753=ORIENTED_EDGE('',*,*,#8356,.T.);
#11754=ORIENTED_EDGE('',*,*,#8382,.T.);
#11755=ORIENTED_EDGE('',*,*,#8386,.T.);
#11756=ORIENTED_EDGE('',*,*,#8371,.T.);
#11757=ORIENTED_EDGE('',*,*,#8377,.T.);
#11758=ORIENTED_EDGE('',*,*,#8383,.F.);
#11759=ORIENTED_EDGE('',*,*,#8387,.T.);
#11760=ORIENTED_EDGE('',*,*,#8385,.T.);
#11761=ORIENTED_EDGE('',*,*,#8387,.F.);
#11762=ORIENTED_EDGE('',*,*,#8379,.T.);
#11763=ORIENTED_EDGE('',*,*,#8384,.F.);
#11764=ORIENTED_EDGE('',*,*,#8374,.T.);
#11765=ORIENTED_EDGE('',*,*,#8388,.T.);
#11766=ORIENTED_EDGE('',*,*,#8363,.T.);
#11767=ORIENTED_EDGE('',*,*,#8368,.T.);
#11768=ORIENTED_EDGE('',*,*,#8361,.T.);
#11769=ORIENTED_EDGE('',*,*,#8364,.T.);
#11770=ORIENTED_EDGE('',*,*,#8359,.T.);
#11771=ORIENTED_EDGE('',*,*,#8381,.T.);
#11772=ORIENTED_EDGE('',*,*,#8389,.T.);
#11773=ORIENTED_EDGE('',*,*,#8372,.T.);
#11774=ORIENTED_EDGE('',*,*,#8386,.F.);
#11775=ORIENTED_EDGE('',*,*,#8366,.T.);
#11776=ORIENTED_EDGE('',*,*,#8367,.T.);
#11777=ORIENTED_EDGE('',*,*,#8380,.T.);
#11778=ORIENTED_EDGE('',*,*,#8388,.F.);
#11779=ORIENTED_EDGE('',*,*,#8373,.T.);
#11780=ORIENTED_EDGE('',*,*,#8389,.F.);
#11781=ORIENTED_EDGE('',*,*,#8390,.F.);
#11782=ORIENTED_EDGE('',*,*,#8391,.T.);
#11783=ORIENTED_EDGE('',*,*,#8392,.T.);
#11784=ORIENTED_EDGE('',*,*,#8391,.F.);
#11785=ORIENTED_EDGE('',*,*,#8393,.F.);
#11786=ORIENTED_EDGE('',*,*,#8394,.T.);
#11787=ORIENTED_EDGE('',*,*,#8395,.T.);
#11788=ORIENTED_EDGE('',*,*,#8394,.F.);
#11789=ORIENTED_EDGE('',*,*,#8393,.T.);
#11790=ORIENTED_EDGE('',*,*,#8390,.T.);
#11791=ORIENTED_EDGE('',*,*,#8395,.F.);
#11792=ORIENTED_EDGE('',*,*,#8392,.F.);
#11793=ORIENTED_EDGE('',*,*,#8396,.F.);
#11794=ORIENTED_EDGE('',*,*,#8397,.T.);
#11795=ORIENTED_EDGE('',*,*,#8398,.T.);
#11796=ORIENTED_EDGE('',*,*,#8397,.F.);
#11797=ORIENTED_EDGE('',*,*,#8399,.F.);
#11798=ORIENTED_EDGE('',*,*,#8400,.T.);
#11799=ORIENTED_EDGE('',*,*,#8401,.T.);
#11800=ORIENTED_EDGE('',*,*,#8400,.F.);
#11801=ORIENTED_EDGE('',*,*,#8399,.T.);
#11802=ORIENTED_EDGE('',*,*,#8396,.T.);
#11803=ORIENTED_EDGE('',*,*,#8401,.F.);
#11804=ORIENTED_EDGE('',*,*,#8398,.F.);
#11805=ORIENTED_EDGE('',*,*,#8402,.F.);
#11806=ORIENTED_EDGE('',*,*,#8403,.F.);
#11807=ORIENTED_EDGE('',*,*,#8404,.F.);
#11808=ORIENTED_EDGE('',*,*,#8405,.F.);
#11809=ORIENTED_EDGE('',*,*,#8406,.F.);
#11810=ORIENTED_EDGE('',*,*,#8407,.F.);
#11811=ORIENTED_EDGE('',*,*,#8408,.F.);
#11812=ORIENTED_EDGE('',*,*,#8409,.F.);
#11813=ORIENTED_EDGE('',*,*,#8406,.T.);
#11814=ORIENTED_EDGE('',*,*,#8410,.T.);
#11815=ORIENTED_EDGE('',*,*,#8411,.T.);
#11816=ORIENTED_EDGE('',*,*,#8412,.T.);
#11817=ORIENTED_EDGE('',*,*,#8405,.T.);
#11818=ORIENTED_EDGE('',*,*,#8413,.F.);
#11819=ORIENTED_EDGE('',*,*,#8414,.T.);
#11820=ORIENTED_EDGE('',*,*,#8410,.F.);
#11821=ORIENTED_EDGE('',*,*,#8404,.T.);
#11822=ORIENTED_EDGE('',*,*,#8415,.T.);
#11823=ORIENTED_EDGE('',*,*,#8416,.T.);
#11824=ORIENTED_EDGE('',*,*,#8413,.T.);
#11825=ORIENTED_EDGE('',*,*,#8403,.T.);
#11826=ORIENTED_EDGE('',*,*,#8417,.F.);
#11827=ORIENTED_EDGE('',*,*,#8418,.T.);
#11828=ORIENTED_EDGE('',*,*,#8415,.F.);
#11829=ORIENTED_EDGE('',*,*,#8419,.F.);
#11830=ORIENTED_EDGE('',*,*,#8420,.F.);
#11831=ORIENTED_EDGE('',*,*,#8411,.F.);
#11832=ORIENTED_EDGE('',*,*,#8414,.F.);
#11833=ORIENTED_EDGE('',*,*,#8416,.F.);
#11834=ORIENTED_EDGE('',*,*,#8418,.F.);
#11835=ORIENTED_EDGE('',*,*,#8421,.F.);
#11836=ORIENTED_EDGE('',*,*,#8422,.F.);
#11837=ORIENTED_EDGE('',*,*,#8407,.T.);
#11838=ORIENTED_EDGE('',*,*,#8412,.F.);
#11839=ORIENTED_EDGE('',*,*,#8420,.T.);
#11840=ORIENTED_EDGE('',*,*,#8423,.F.);
#11841=ORIENTED_EDGE('',*,*,#8402,.T.);
#11842=ORIENTED_EDGE('',*,*,#8424,.T.);
#11843=ORIENTED_EDGE('',*,*,#8421,.T.);
#11844=ORIENTED_EDGE('',*,*,#8417,.T.);
#11845=ORIENTED_EDGE('',*,*,#8408,.T.);
#11846=ORIENTED_EDGE('',*,*,#8423,.T.);
#11847=ORIENTED_EDGE('',*,*,#8419,.T.);
#11848=ORIENTED_EDGE('',*,*,#8425,.T.);
#11849=ORIENTED_EDGE('',*,*,#8409,.T.);
#11850=ORIENTED_EDGE('',*,*,#8425,.F.);
#11851=ORIENTED_EDGE('',*,*,#8422,.T.);
#11852=ORIENTED_EDGE('',*,*,#8424,.F.);
#11853=ORIENTED_EDGE('',*,*,#8426,.F.);
#11854=ORIENTED_EDGE('',*,*,#8427,.T.);
#11855=ORIENTED_EDGE('',*,*,#8428,.T.);
#11856=ORIENTED_EDGE('',*,*,#8429,.F.);
#11857=ORIENTED_EDGE('',*,*,#8430,.F.);
#11858=ORIENTED_EDGE('',*,*,#8431,.T.);
#11859=ORIENTED_EDGE('',*,*,#8432,.T.);
#11860=ORIENTED_EDGE('',*,*,#8427,.F.);
#11861=ORIENTED_EDGE('',*,*,#8433,.F.);
#11862=ORIENTED_EDGE('',*,*,#8434,.T.);
#11863=ORIENTED_EDGE('',*,*,#8435,.T.);
#11864=ORIENTED_EDGE('',*,*,#8431,.F.);
#11865=ORIENTED_EDGE('',*,*,#8436,.F.);
#11866=ORIENTED_EDGE('',*,*,#8437,.T.);
#11867=ORIENTED_EDGE('',*,*,#8438,.T.);
#11868=ORIENTED_EDGE('',*,*,#8434,.F.);
#11869=ORIENTED_EDGE('',*,*,#8439,.F.);
#11870=ORIENTED_EDGE('',*,*,#8440,.T.);
#11871=ORIENTED_EDGE('',*,*,#8441,.T.);
#11872=ORIENTED_EDGE('',*,*,#8437,.F.);
#11873=ORIENTED_EDGE('',*,*,#8442,.F.);
#11874=ORIENTED_EDGE('',*,*,#8429,.T.);
#11875=ORIENTED_EDGE('',*,*,#8443,.T.);
#11876=ORIENTED_EDGE('',*,*,#8440,.F.);
#11877=ORIENTED_EDGE('',*,*,#8443,.F.);
#11878=ORIENTED_EDGE('',*,*,#8428,.F.);
#11879=ORIENTED_EDGE('',*,*,#8432,.F.);
#11880=ORIENTED_EDGE('',*,*,#8435,.F.);
#11881=ORIENTED_EDGE('',*,*,#8438,.F.);
#11882=ORIENTED_EDGE('',*,*,#8441,.F.);
#11883=ORIENTED_EDGE('',*,*,#8444,.F.);
#11884=ORIENTED_EDGE('',*,*,#8426,.T.);
#11885=ORIENTED_EDGE('',*,*,#8442,.T.);
#11886=ORIENTED_EDGE('',*,*,#8439,.T.);
#11887=ORIENTED_EDGE('',*,*,#8436,.T.);
#11888=ORIENTED_EDGE('',*,*,#8433,.T.);
#11889=ORIENTED_EDGE('',*,*,#8430,.T.);
#11890=ORIENTED_EDGE('',*,*,#8445,.F.);
#11891=ORIENTED_EDGE('',*,*,#8446,.T.);
#11892=ORIENTED_EDGE('',*,*,#8444,.T.);
#11893=ORIENTED_EDGE('',*,*,#8446,.F.);
#11894=ORIENTED_EDGE('',*,*,#8447,.F.);
#11895=ORIENTED_EDGE('',*,*,#8448,.T.);
#11896=ORIENTED_EDGE('',*,*,#8445,.T.);
#11897=ORIENTED_EDGE('',*,*,#8448,.F.);
#11898=ORIENTED_EDGE('',*,*,#8449,.F.);
#11899=ORIENTED_EDGE('',*,*,#8450,.T.);
#11900=ORIENTED_EDGE('',*,*,#8447,.T.);
#11901=ORIENTED_EDGE('',*,*,#8450,.F.);
#11902=ORIENTED_EDGE('',*,*,#8449,.T.);
#11903=ORIENTED_EDGE('',*,*,#8451,.F.);
#11904=ORIENTED_EDGE('',*,*,#8452,.T.);
#11905=ORIENTED_EDGE('',*,*,#8453,.T.);
#11906=ORIENTED_EDGE('',*,*,#8452,.F.);
#11907=ORIENTED_EDGE('',*,*,#8454,.F.);
#11908=ORIENTED_EDGE('',*,*,#8455,.T.);
#11909=ORIENTED_EDGE('',*,*,#8456,.T.);
#11910=ORIENTED_EDGE('',*,*,#8455,.F.);
#11911=ORIENTED_EDGE('',*,*,#8454,.T.);
#11912=ORIENTED_EDGE('',*,*,#8451,.T.);
#11913=ORIENTED_EDGE('',*,*,#8456,.F.);
#11914=ORIENTED_EDGE('',*,*,#8453,.F.);
#11915=ORIENTED_EDGE('',*,*,#8457,.F.);
#11916=ORIENTED_EDGE('',*,*,#8458,.F.);
#11917=ORIENTED_EDGE('',*,*,#8459,.T.);
#11918=ORIENTED_EDGE('',*,*,#8457,.T.);
#11919=ORIENTED_EDGE('',*,*,#8459,.F.);
#11920=ORIENTED_EDGE('',*,*,#8460,.F.);
#11921=ORIENTED_EDGE('',*,*,#8461,.T.);
#11922=ORIENTED_EDGE('',*,*,#8458,.T.);
#11923=ORIENTED_EDGE('',*,*,#8461,.F.);
#11924=ORIENTED_EDGE('',*,*,#8462,.F.);
#11925=ORIENTED_EDGE('',*,*,#8463,.T.);
#11926=ORIENTED_EDGE('',*,*,#8460,.T.);
#11927=ORIENTED_EDGE('',*,*,#8463,.F.);
#11928=ORIENTED_EDGE('',*,*,#8462,.T.);
#11929=ORIENTED_EDGE('',*,*,#8464,.F.);
#11930=ORIENTED_EDGE('',*,*,#8465,.F.);
#11931=ORIENTED_EDGE('',*,*,#8466,.T.);
#11932=ORIENTED_EDGE('',*,*,#8464,.T.);
#11933=ORIENTED_EDGE('',*,*,#8466,.F.);
#11934=ORIENTED_EDGE('',*,*,#8467,.F.);
#11935=ORIENTED_EDGE('',*,*,#8468,.T.);
#11936=ORIENTED_EDGE('',*,*,#8465,.T.);
#11937=ORIENTED_EDGE('',*,*,#8468,.F.);
#11938=ORIENTED_EDGE('',*,*,#8469,.F.);
#11939=ORIENTED_EDGE('',*,*,#8470,.T.);
#11940=ORIENTED_EDGE('',*,*,#8467,.T.);
#11941=ORIENTED_EDGE('',*,*,#8470,.F.);
#11942=ORIENTED_EDGE('',*,*,#8469,.T.);
#11943=ORIENTED_EDGE('',*,*,#8471,.T.);
#11944=ORIENTED_EDGE('',*,*,#8472,.T.);
#11945=ORIENTED_EDGE('',*,*,#8473,.T.);
#11946=ORIENTED_EDGE('',*,*,#8474,.F.);
#11947=ORIENTED_EDGE('',*,*,#8475,.T.);
#11948=ORIENTED_EDGE('',*,*,#8476,.T.);
#11949=ORIENTED_EDGE('',*,*,#8477,.T.);
#11950=ORIENTED_EDGE('',*,*,#8472,.F.);
#11951=ORIENTED_EDGE('',*,*,#8478,.T.);
#11952=ORIENTED_EDGE('',*,*,#8479,.T.);
#11953=ORIENTED_EDGE('',*,*,#8480,.T.);
#11954=ORIENTED_EDGE('',*,*,#8476,.F.);
#11955=ORIENTED_EDGE('',*,*,#8481,.T.);
#11956=ORIENTED_EDGE('',*,*,#8482,.T.);
#11957=ORIENTED_EDGE('',*,*,#8483,.T.);
#11958=ORIENTED_EDGE('',*,*,#8479,.F.);
#11959=ORIENTED_EDGE('',*,*,#8484,.T.);
#11960=ORIENTED_EDGE('',*,*,#8485,.T.);
#11961=ORIENTED_EDGE('',*,*,#8486,.T.);
#11962=ORIENTED_EDGE('',*,*,#8482,.F.);
#11963=ORIENTED_EDGE('',*,*,#8487,.T.);
#11964=ORIENTED_EDGE('',*,*,#8474,.T.);
#11965=ORIENTED_EDGE('',*,*,#8488,.T.);
#11966=ORIENTED_EDGE('',*,*,#8485,.F.);
#11967=ORIENTED_EDGE('',*,*,#8487,.F.);
#11968=ORIENTED_EDGE('',*,*,#8484,.F.);
#11969=ORIENTED_EDGE('',*,*,#8481,.F.);
#11970=ORIENTED_EDGE('',*,*,#8478,.F.);
#11971=ORIENTED_EDGE('',*,*,#8475,.F.);
#11972=ORIENTED_EDGE('',*,*,#8471,.F.);
#11973=ORIENTED_EDGE('',*,*,#8488,.F.);
#11974=ORIENTED_EDGE('',*,*,#8473,.F.);
#11975=ORIENTED_EDGE('',*,*,#8477,.F.);
#11976=ORIENTED_EDGE('',*,*,#8480,.F.);
#11977=ORIENTED_EDGE('',*,*,#8483,.F.);
#11978=ORIENTED_EDGE('',*,*,#8486,.F.);
#11979=CYLINDRICAL_SURFACE('',#13562,0.274999999999999);
#11980=CYLINDRICAL_SURFACE('',#13565,0.275);
#11981=CYLINDRICAL_SURFACE('',#13568,0.275);
#11982=CYLINDRICAL_SURFACE('',#13571,0.274999999999999);
#11983=CYLINDRICAL_SURFACE('',#13574,0.210000000000001);
#11984=CYLINDRICAL_SURFACE('',#13577,0.210000000000001);
#11985=CYLINDRICAL_SURFACE('',#13580,0.21);
#11986=CYLINDRICAL_SURFACE('',#13583,0.21);
#11987=CYLINDRICAL_SURFACE('',#13586,0.329999999999998);
#11988=CYLINDRICAL_SURFACE('',#13589,0.329999999999998);
#11989=CYLINDRICAL_SURFACE('',#13592,0.275);
#11990=CYLINDRICAL_SURFACE('',#13595,0.275);
#11991=CYLINDRICAL_SURFACE('',#13598,0.210000000000001);
#11992=CYLINDRICAL_SURFACE('',#13601,0.21);
#11993=CYLINDRICAL_SURFACE('',#13604,0.21);
#11994=CYLINDRICAL_SURFACE('',#13607,0.210000000000001);
#11995=CYLINDRICAL_SURFACE('',#13617,0.164999999999999);
#11996=CYLINDRICAL_SURFACE('',#13620,0.164999999999999);
#11997=CYLINDRICAL_SURFACE('',#13623,0.165);
#11998=CYLINDRICAL_SURFACE('',#13626,0.164999999999999);
#11999=CYLINDRICAL_SURFACE('',#13629,0.5);
#12000=CYLINDRICAL_SURFACE('',#13634,0.5);
#12001=CYLINDRICAL_SURFACE('',#13639,0.5);
#12002=CYLINDRICAL_SURFACE('',#13644,0.5);
#12003=CYLINDRICAL_SURFACE('',#13649,0.274999999999999);
#12004=CYLINDRICAL_SURFACE('',#13651,0.275);
#12005=CYLINDRICAL_SURFACE('',#13653,0.275);
#12006=CYLINDRICAL_SURFACE('',#13655,0.274999999999999);
#12007=CYLINDRICAL_SURFACE('',#13664,0.165);
#12008=CYLINDRICAL_SURFACE('',#13667,0.165);
#12009=CYLINDRICAL_SURFACE('',#13670,0.165);
#12010=CYLINDRICAL_SURFACE('',#13673,1.6);
#12011=CYLINDRICAL_SURFACE('',#13678,1.4);
#12012=CYLINDRICAL_SURFACE('',#13680,0.21);
#12013=CYLINDRICAL_SURFACE('',#13684,0.21);
#12014=CYLINDRICAL_SURFACE('',#13695,0.225);
#12015=CYLINDRICAL_SURFACE('',#13698,0.225);
#12016=CYLINDRICAL_SURFACE('',#13701,0.225);
#12017=CYLINDRICAL_SURFACE('',#13704,1.59);
#12018=CYLINDRICAL_SURFACE('',#13709,1.2);
#12019=CYLINDRICAL_SURFACE('',#13711,2.4);
#12020=CYLINDRICAL_SURFACE('',#13717,0.165);
#12021=CYLINDRICAL_SURFACE('',#13720,0.165);
#12022=CYLINDRICAL_SURFACE('',#13723,0.165);
#12023=CYLINDRICAL_SURFACE('',#13726,2.35);
#12024=CYLINDRICAL_SURFACE('',#13731,2.15);
#12025=CYLINDRICAL_SURFACE('',#13733,0.25);
#12026=CYLINDRICAL_SURFACE('',#13737,0.25);
#12027=CYLINDRICAL_SURFACE('',#13755,3.);
#12028=CYLINDRICAL_SURFACE('',#13757,0.225);
#12029=CYLINDRICAL_SURFACE('',#13759,0.225);
#12030=CYLINDRICAL_SURFACE('',#13761,0.225);
#12031=CYLINDRICAL_SURFACE('',#13763,2.34);
#12032=CYLINDRICAL_SURFACE('',#13767,1.8);
#12033=CYLINDRICAL_SURFACE('',#13775,0.475);
#12034=CYLINDRICAL_SURFACE('',#13782,0.475);
#12035=CYLINDRICAL_SURFACE('',#13787,0.275);
#12036=CYLINDRICAL_SURFACE('',#13789,0.275);
#12037=CYLINDRICAL_SURFACE('',#13804,0.475000000000001);
#12038=CYLINDRICAL_SURFACE('',#13811,0.475000000000001);
#12039=CYLINDRICAL_SURFACE('',#13816,0.274999999999999);
#12040=CYLINDRICAL_SURFACE('',#13818,0.274999999999999);
#12041=CYLINDRICAL_SURFACE('',#13829,0.375);
#12042=CYLINDRICAL_SURFACE('',#13834,0.375);
#12043=CYLINDRICAL_SURFACE('',#13839,0.375);
#12044=CYLINDRICAL_SURFACE('',#13844,0.375);
#12045=CYLINDRICAL_SURFACE('',#13849,0.225);
#12046=CYLINDRICAL_SURFACE('',#13851,0.225);
#12047=CYLINDRICAL_SURFACE('',#13853,0.225);
#12048=CYLINDRICAL_SURFACE('',#13855,0.225000000000001);
#12049=CYLINDRICAL_SURFACE('',#13879,1.070235);
#12050=CYLINDRICAL_SURFACE('',#13881,0.6);
#12051=CYLINDRICAL_SURFACE('',#13887,1.070235);
#12052=CYLINDRICAL_SURFACE('',#13899,1.129765);
#12053=CYLINDRICAL_SURFACE('',#13906,1.6);
#12054=CYLINDRICAL_SURFACE('',#13911,1.129765);
#12055=CYLINDRICAL_SURFACE('',#13931,1.123812);
#12056=CYLINDRICAL_SURFACE('',#13967,1.076188);
#12057=CYLINDRICAL_SURFACE('',#13981,1.119765);
#12058=CYLINDRICAL_SURFACE('',#13985,1.085235);
#12059=CYLINDRICAL_SURFACE('',#13989,1.119765);
#12060=CYLINDRICAL_SURFACE('',#13993,1.085235);
#12061=CYLINDRICAL_SURFACE('',#14007,1.63531);
#12062=CYLINDRICAL_SURFACE('',#14009,1.);
#12063=CYLINDRICAL_SURFACE('',#14015,1.63531);
#12064=CYLINDRICAL_SURFACE('',#14027,1.71469);
#12065=CYLINDRICAL_SURFACE('',#14034,2.35);
#12066=CYLINDRICAL_SURFACE('',#14039,1.71469);
#12067=CYLINDRICAL_SURFACE('',#14061,1.706752);
#12068=CYLINDRICAL_SURFACE('',#14101,1.643248);
#12069=CYLINDRICAL_SURFACE('',#14115,1.70469);
#12070=CYLINDRICAL_SURFACE('',#14119,1.65031);
#12071=CYLINDRICAL_SURFACE('',#14123,1.70469);
#12072=CYLINDRICAL_SURFACE('',#14127,1.65031);
#12073=CYLINDRICAL_SURFACE('',#14170,0.21);
#12074=CYLINDRICAL_SURFACE('',#14186,0.2117);
#12075=CYLINDRICAL_SURFACE('',#14204,0.265);
#12076=CYLINDRICAL_SURFACE('',#14208,0.5);
#12077=CYLINDRICAL_SURFACE('',#14226,0.425);
#12078=CYLINDRICAL_SURFACE('',#14234,0.24505);
#12079=CYLINDRICAL_SURFACE('',#14237,0.275);
#12080=CYLINDRICAL_SURFACE('',#14240,0.275);
#12081=CYLINDRICAL_SURFACE('',#14243,0.275);
#12082=CYLINDRICAL_SURFACE('',#14246,0.275);
#12083=CYLINDRICAL_SURFACE('',#14256,0.275);
#12084=CYLINDRICAL_SURFACE('',#14259,0.275);
#12085=CYLINDRICAL_SURFACE('',#14262,0.275);
#12086=CYLINDRICAL_SURFACE('',#14265,0.275);
#12087=CYLINDRICAL_SURFACE('',#14268,0.275);
#12088=CYLINDRICAL_SURFACE('',#14271,0.275);
#12089=CYLINDRICAL_SURFACE('',#14274,0.275);
#12090=CYLINDRICAL_SURFACE('',#14277,0.275);
#12091=CYLINDRICAL_SURFACE('',#14287,0.210000000000001);
#12092=CYLINDRICAL_SURFACE('',#14291,0.210000000000001);
#12093=CYLINDRICAL_SURFACE('',#14295,0.210000000000001);
#12094=CYLINDRICAL_SURFACE('',#14299,0.210000000000001);
#12095=CYLINDRICAL_SURFACE('',#14303,0.165);
#12096=CYLINDRICAL_SURFACE('',#14307,0.165);
#12097=CYLINDRICAL_SURFACE('',#14311,0.165);
#12098=CYLINDRICAL_SURFACE('',#14315,1.11);
#12099=CYLINDRICAL_SURFACE('',#14328,0.21);
#12100=CYLINDRICAL_SURFACE('',#14334,0.21);
#12101=CYLINDRICAL_SURFACE('',#14340,0.21);
#12102=CYLINDRICAL_SURFACE('',#14346,0.21);
#12103=CYLINDRICAL_SURFACE('',#14393,0.265);
#12104=CYLINDRICAL_SURFACE('',#14397,0.5);
#12105=CYLINDRICAL_SURFACE('',#14412,0.25);
#12106=CYLINDRICAL_SURFACE('',#14419,0.425);
#12107=CYLINDRICAL_SURFACE('',#14427,0.24505);
#12108=CYLINDRICAL_SURFACE('',#14429,0.457875);
#12109=CYLINDRICAL_SURFACE('',#14431,0.457875);
#12110=CYLINDRICAL_SURFACE('',#14432,0.457875);
#12111=CYLINDRICAL_SURFACE('',#14433,0.457875);
#12112=CYLINDRICAL_SURFACE('',#14434,0.457875);
#12113=CYLINDRICAL_SURFACE('',#14435,0.457875);
#12114=CYLINDRICAL_SURFACE('',#14436,0.457875);
#12115=CYLINDRICAL_SURFACE('',#14437,0.457875);
#12116=CYLINDRICAL_SURFACE('',#14438,0.457875);
#12117=CYLINDRICAL_SURFACE('',#14440,0.625);
#12118=CYLINDRICAL_SURFACE('',#14442,0.625);
#12119=CYLINDRICAL_SURFACE('',#14443,0.625);
#12120=CYLINDRICAL_SURFACE('',#14444,0.625);
#12121=CYLINDRICAL_SURFACE('',#14445,0.625);
#12122=CYLINDRICAL_SURFACE('',#14446,0.625);
#12123=CYLINDRICAL_SURFACE('',#14447,0.625);
#12124=CYLINDRICAL_SURFACE('',#14448,0.625);
#12125=CYLINDRICAL_SURFACE('',#14449,0.625);
#12126=CYLINDRICAL_SURFACE('',#14451,0.625);
#12127=CYLINDRICAL_SURFACE('',#14458,0.225);
#12128=CYLINDRICAL_SURFACE('',#14460,0.225);
#12129=CYLINDRICAL_SURFACE('',#14462,0.225);
#12130=CYLINDRICAL_SURFACE('',#14468,1.9);
#12131=CYLINDRICAL_SURFACE('',#14469,0.457875);
#12132=CYLINDRICAL_SURFACE('',#14470,1.1);
#12133=CYLINDRICAL_SURFACE('',#14478,0.35);
#12134=CYLINDRICAL_SURFACE('',#14486,0.1954);
#12135=CYLINDRICAL_SURFACE('',#14504,0.425);
#12136=CYLINDRICAL_SURFACE('',#14512,0.24505);
#12137=CYLINDRICAL_SURFACE('',#14547,0.5941);
#12138=CYLINDRICAL_SURFACE('',#14549,0.5941);
#12139=CYLINDRICAL_SURFACE('',#14550,0.5941);
#12140=CYLINDRICAL_SURFACE('',#14551,0.5941);
#12141=CYLINDRICAL_SURFACE('',#14552,0.5941);
#12142=CYLINDRICAL_SURFACE('',#14553,0.5941);
#12143=CYLINDRICAL_SURFACE('',#14554,0.5941);
#12144=CYLINDRICAL_SURFACE('',#14555,0.5941);
#12145=CYLINDRICAL_SURFACE('',#14556,0.5941);
#12146=CYLINDRICAL_SURFACE('',#14557,0.5941);
#12147=CYLINDRICAL_SURFACE('',#14558,0.5941);
#12148=CYLINDRICAL_SURFACE('',#14559,0.5941);
#12149=CYLINDRICAL_SURFACE('',#14560,0.5941);
#12150=CYLINDRICAL_SURFACE('',#14561,0.5941);
#12151=CYLINDRICAL_SURFACE('',#14562,0.5941);
#12152=CYLINDRICAL_SURFACE('',#14563,0.5941);
#12153=CYLINDRICAL_SURFACE('',#14564,0.5941);
#12154=CYLINDRICAL_SURFACE('',#14565,0.5941);
#12155=CYLINDRICAL_SURFACE('',#14566,0.5941);
#12156=CYLINDRICAL_SURFACE('',#14567,0.5941);
#12157=CYLINDRICAL_SURFACE('',#14568,0.5941);
#12158=CYLINDRICAL_SURFACE('',#14569,0.5941);
#12159=CYLINDRICAL_SURFACE('',#14570,0.5941);
#12160=CYLINDRICAL_SURFACE('',#14571,0.5941);
#12161=CYLINDRICAL_SURFACE('',#14572,0.5941);
#12162=CYLINDRICAL_SURFACE('',#14573,0.5941);
#12163=CYLINDRICAL_SURFACE('',#14574,0.5941);
#12164=CYLINDRICAL_SURFACE('',#14575,0.5941);
#12165=CYLINDRICAL_SURFACE('',#14576,0.5941);
#12166=CYLINDRICAL_SURFACE('',#14577,0.5941);
#12167=CYLINDRICAL_SURFACE('',#14578,0.5941);
#12168=CYLINDRICAL_SURFACE('',#14579,0.5941);
#12169=CYLINDRICAL_SURFACE('',#14580,0.5941);
#12170=CYLINDRICAL_SURFACE('',#14581,0.5941);
#12171=CYLINDRICAL_SURFACE('',#14582,0.5941);
#12172=CYLINDRICAL_SURFACE('',#14583,0.5941);
#12173=CYLINDRICAL_SURFACE('',#14584,0.5941);
#12174=CYLINDRICAL_SURFACE('',#14585,0.5941);
#12175=CYLINDRICAL_SURFACE('',#14586,0.5941);
#12176=CYLINDRICAL_SURFACE('',#14587,0.5941);
#12177=CYLINDRICAL_SURFACE('',#14588,0.5941);
#12178=CYLINDRICAL_SURFACE('',#14589,0.5941);
#12179=CYLINDRICAL_SURFACE('',#14590,0.5941);
#12180=CYLINDRICAL_SURFACE('',#14591,0.5941);
#12181=CYLINDRICAL_SURFACE('',#14592,0.5941);
#12182=CYLINDRICAL_SURFACE('',#14593,0.5941);
#12183=CYLINDRICAL_SURFACE('',#14594,0.5941);
#12184=CYLINDRICAL_SURFACE('',#14595,0.5941);
#12185=CYLINDRICAL_SURFACE('',#14596,0.5941);
#12186=CYLINDRICAL_SURFACE('',#14597,0.5941);
#12187=CYLINDRICAL_SURFACE('',#14598,0.5941);
#12188=CYLINDRICAL_SURFACE('',#14599,0.5941);
#12189=CYLINDRICAL_SURFACE('',#14600,0.5941);
#12190=CYLINDRICAL_SURFACE('',#14601,0.5941);
#12191=CYLINDRICAL_SURFACE('',#14602,0.5941);
#12192=CYLINDRICAL_SURFACE('',#14603,0.5941);
#12193=CYLINDRICAL_SURFACE('',#14604,0.5941);
#12194=CYLINDRICAL_SURFACE('',#14605,0.5941);
#12195=CYLINDRICAL_SURFACE('',#14606,0.5941);
#12196=CYLINDRICAL_SURFACE('',#14607,0.5941);
#12197=CYLINDRICAL_SURFACE('',#14608,0.5941);
#12198=CYLINDRICAL_SURFACE('',#14609,0.5941);
#12199=CYLINDRICAL_SURFACE('',#14610,0.5941);
#12200=CYLINDRICAL_SURFACE('',#14611,0.415875);
#12201=CYLINDRICAL_SURFACE('',#14613,0.415875);
#12202=CYLINDRICAL_SURFACE('',#14615,0.415875);
#12203=CYLINDRICAL_SURFACE('',#14616,0.415875);
#12204=CYLINDRICAL_SURFACE('',#14617,0.415875);
#12205=CYLINDRICAL_SURFACE('',#14618,0.415875);
#12206=CYLINDRICAL_SURFACE('',#14619,0.415875);
#12207=CYLINDRICAL_SURFACE('',#14620,0.415875);
#12208=CYLINDRICAL_SURFACE('',#14621,0.415875);
#12209=CYLINDRICAL_SURFACE('',#14622,0.415875);
#12210=CYLINDRICAL_SURFACE('',#14623,0.415875);
#12211=CYLINDRICAL_SURFACE('',#14624,0.415875);
#12212=CYLINDRICAL_SURFACE('',#14625,0.415875);
#12213=CYLINDRICAL_SURFACE('',#14626,0.415875);
#12214=CYLINDRICAL_SURFACE('',#14627,0.415875);
#12215=CYLINDRICAL_SURFACE('',#14628,0.415875);
#12216=CYLINDRICAL_SURFACE('',#14629,0.415875);
#12217=CYLINDRICAL_SURFACE('',#14630,0.415875);
#12218=CYLINDRICAL_SURFACE('',#14631,0.415875);
#12219=CYLINDRICAL_SURFACE('',#14632,0.415875);
#12220=CYLINDRICAL_SURFACE('',#14633,0.415875);
#12221=CYLINDRICAL_SURFACE('',#14634,0.415875);
#12222=CYLINDRICAL_SURFACE('',#14635,0.415875);
#12223=CYLINDRICAL_SURFACE('',#14636,0.415875);
#12224=CYLINDRICAL_SURFACE('',#14637,0.415875);
#12225=CYLINDRICAL_SURFACE('',#14638,0.415875);
#12226=CYLINDRICAL_SURFACE('',#14639,0.415875);
#12227=CYLINDRICAL_SURFACE('',#14640,0.415875);
#12228=CYLINDRICAL_SURFACE('',#14641,0.415875);
#12229=CYLINDRICAL_SURFACE('',#14642,0.415875);
#12230=CYLINDRICAL_SURFACE('',#14643,0.415875);
#12231=CYLINDRICAL_SURFACE('',#14644,0.415875);
#12232=CYLINDRICAL_SURFACE('',#14645,0.415875);
#12233=CYLINDRICAL_SURFACE('',#14646,0.415875);
#12234=CYLINDRICAL_SURFACE('',#14647,0.415875);
#12235=CYLINDRICAL_SURFACE('',#14648,0.415875);
#12236=CYLINDRICAL_SURFACE('',#14649,0.415875);
#12237=CYLINDRICAL_SURFACE('',#14650,0.415875);
#12238=CYLINDRICAL_SURFACE('',#14651,0.415875);
#12239=CYLINDRICAL_SURFACE('',#14652,0.415875);
#12240=CYLINDRICAL_SURFACE('',#14653,0.415875);
#12241=CYLINDRICAL_SURFACE('',#14654,0.415875);
#12242=CYLINDRICAL_SURFACE('',#14655,0.415875);
#12243=CYLINDRICAL_SURFACE('',#14656,0.415875);
#12244=CYLINDRICAL_SURFACE('',#14657,0.415875);
#12245=CYLINDRICAL_SURFACE('',#14658,0.415875);
#12246=CYLINDRICAL_SURFACE('',#14659,0.415875);
#12247=CYLINDRICAL_SURFACE('',#14660,0.415875);
#12248=CYLINDRICAL_SURFACE('',#14661,0.415875);
#12249=CYLINDRICAL_SURFACE('',#14662,0.415875);
#12250=CYLINDRICAL_SURFACE('',#14663,0.415875);
#12251=CYLINDRICAL_SURFACE('',#14664,0.415875);
#12252=CYLINDRICAL_SURFACE('',#14665,0.415875);
#12253=CYLINDRICAL_SURFACE('',#14666,0.415875);
#12254=CYLINDRICAL_SURFACE('',#14667,0.415875);
#12255=CYLINDRICAL_SURFACE('',#14668,0.415875);
#12256=CYLINDRICAL_SURFACE('',#14669,0.415875);
#12257=CYLINDRICAL_SURFACE('',#14670,0.415875);
#12258=CYLINDRICAL_SURFACE('',#14671,0.415875);
#12259=CYLINDRICAL_SURFACE('',#14672,0.415875);
#12260=CYLINDRICAL_SURFACE('',#14673,0.415875);
#12261=CYLINDRICAL_SURFACE('',#14674,0.415875);
#12262=CYLINDRICAL_SURFACE('',#14675,0.415875);
#12263=CYLINDRICAL_SURFACE('',#14679,0.6);
#12264=CYLINDRICAL_SURFACE('',#14682,0.415875);
#12265=CYLINDRICAL_SURFACE('',#14690,1.);
#12266=CYLINDRICAL_SURFACE('',#14697,1.35);
#12267=CYLINDRICAL_SURFACE('',#14700,0.5941);
#12268=CYLINDRICAL_SURFACE('',#14702,1.01);
#12269=CYLINDRICAL_SURFACE('',#14705,1.35);
#12270=CYLINDRICAL_SURFACE('',#14713,0.210000000000001);
#12271=CYLINDRICAL_SURFACE('',#14716,1.005);
#12272=CYLINDRICAL_SURFACE('',#14719,1.5);
#12273=CYLINDRICAL_SURFACE('',#14725,0.25);
#12274=CYLINDRICAL_SURFACE('',#14730,0.210000000000001);
#12275=CYLINDRICAL_SURFACE('',#14742,3.5);
#12276=CYLINDRICAL_SURFACE('',#14743,1.);
#12277=CYLINDRICAL_SURFACE('',#14745,1.5);
#12278=CYLINDRICAL_SURFACE('',#14749,0.33);
#12279=CYLINDRICAL_SURFACE('',#14752,0.4);
#12280=CYLINDRICAL_SURFACE('',#14758,0.405);
#12281=CYLINDRICAL_SURFACE('',#14761,0.9);
#12282=CYLINDRICAL_SURFACE('',#14789,0.24505);
#12283=CYLINDRICAL_SURFACE('',#14795,0.32);
#12284=CYLINDRICAL_SURFACE('',#14798,0.6);
#12285=CYLINDRICAL_SURFACE('',#14808,0.5);
#12286=CYLINDRICAL_SURFACE('',#14816,0.2942);
#12287=ADVANCED_FACE('',(#1575),#11979,.F.);
#12288=ADVANCED_FACE('',(#1576),#11980,.F.);
#12289=ADVANCED_FACE('',(#1577),#11981,.F.);
#12290=ADVANCED_FACE('',(#1578),#11982,.F.);
#12291=ADVANCED_FACE('',(#1579),#11983,.F.);
#12292=ADVANCED_FACE('',(#1580),#11984,.F.);
#12293=ADVANCED_FACE('',(#1581),#11985,.F.);
#12294=ADVANCED_FACE('',(#1582),#11986,.F.);
#12295=ADVANCED_FACE('',(#1583),#11987,.F.);
#12296=ADVANCED_FACE('',(#1584),#11988,.F.);
#12297=ADVANCED_FACE('',(#1585),#11989,.F.);
#12298=ADVANCED_FACE('',(#1586),#11990,.F.);
#12299=ADVANCED_FACE('',(#1587),#11991,.F.);
#12300=ADVANCED_FACE('',(#1588),#11992,.F.);
#12301=ADVANCED_FACE('',(#1589),#11993,.F.);
#12302=ADVANCED_FACE('',(#1590),#11994,.F.);
#12303=ADVANCED_FACE('',(#1591),#1228,.T.);
#12304=ADVANCED_FACE('',(#1592),#1229,.T.);
#12305=ADVANCED_FACE('',(#1593),#1230,.T.);
#12306=ADVANCED_FACE('',(#1594),#1231,.T.);
#12307=ADVANCED_FACE('',(#1595,#1012,#1013,#1014,#1015,#1016,#1017,#1018,
#1019,#1020,#1021,#1022,#1023,#1024,#1025,#1026,#1027),#1232,.T.);
#12308=ADVANCED_FACE('',(#1596,#1028,#1029,#1030,#1031,#1032,#1033,#1034,
#1035,#1036,#1037,#1038,#1039,#1040,#1041,#1042,#1043),#1233,.F.);
#12309=ADVANCED_FACE('',(#1597),#11995,.F.);
#12310=ADVANCED_FACE('',(#1598),#11996,.F.);
#12311=ADVANCED_FACE('',(#1599),#11997,.F.);
#12312=ADVANCED_FACE('',(#1600),#11998,.F.);
#12313=ADVANCED_FACE('',(#1601),#11999,.F.);
#12314=ADVANCED_FACE('',(#1602,#1044),#1234,.T.);
#12315=ADVANCED_FACE('',(#1603),#12000,.F.);
#12316=ADVANCED_FACE('',(#1604,#1045),#1235,.T.);
#12317=ADVANCED_FACE('',(#1605),#12001,.F.);
#12318=ADVANCED_FACE('',(#1606,#1046),#1236,.T.);
#12319=ADVANCED_FACE('',(#1607),#12002,.F.);
#12320=ADVANCED_FACE('',(#1608,#1047),#1237,.T.);
#12321=ADVANCED_FACE('',(#1609),#12003,.F.);
#12322=ADVANCED_FACE('',(#1610),#12004,.F.);
#12323=ADVANCED_FACE('',(#1611),#12005,.F.);
#12324=ADVANCED_FACE('',(#1612),#12006,.F.);
#12325=ADVANCED_FACE('',(#1613),#1238,.T.);
#12326=ADVANCED_FACE('',(#1614),#1239,.T.);
#12327=ADVANCED_FACE('',(#1615),#1240,.T.);
#12328=ADVANCED_FACE('',(#1616),#1241,.T.);
#12329=ADVANCED_FACE('',(#1617,#1048,#1049,#1050,#1051,#1052,#1053,#1054,
#1055),#1242,.T.);
#12330=ADVANCED_FACE('',(#1618,#1056,#1057,#1058,#1059,#1060,#1061,#1062,
#1063),#1243,.F.);
#12331=ADVANCED_FACE('',(#1619),#12007,.F.);
#12332=ADVANCED_FACE('',(#1620),#12008,.F.);
#12333=ADVANCED_FACE('',(#1621),#12009,.F.);
#12334=ADVANCED_FACE('',(#1622),#12010,.F.);
#12335=ADVANCED_FACE('',(#1623,#1064),#1244,.F.);
#12336=ADVANCED_FACE('',(#1624),#12011,.F.);
#12337=ADVANCED_FACE('',(#1625),#12012,.F.);
#12338=ADVANCED_FACE('',(#1626),#1245,.F.);
#12339=ADVANCED_FACE('',(#1627),#12013,.F.);
#12340=ADVANCED_FACE('',(#1628),#1246,.F.);
#12341=ADVANCED_FACE('',(#1629),#1247,.T.);
#12342=ADVANCED_FACE('',(#1630,#1065,#1066,#1067,#1068),#1248,.T.);
#12343=ADVANCED_FACE('',(#1631),#1249,.T.);
#12344=ADVANCED_FACE('',(#1632,#1069,#1070,#1071,#1072),#1250,.T.);
#12345=ADVANCED_FACE('',(#1633),#1251,.T.);
#12346=ADVANCED_FACE('',(#1634,#1073,#1074),#1252,.F.);
#12347=ADVANCED_FACE('',(#1635),#12014,.F.);
#12348=ADVANCED_FACE('',(#1636),#12015,.F.);
#12349=ADVANCED_FACE('',(#1637),#12016,.F.);
#12350=ADVANCED_FACE('',(#1638),#12017,.T.);
#12351=ADVANCED_FACE('',(#1639,#1075),#1253,.T.);
#12352=ADVANCED_FACE('',(#1640),#12018,.F.);
#12353=ADVANCED_FACE('',(#1641),#12019,.T.);
#12354=ADVANCED_FACE('',(#1642,#1076,#1077,#1078,#1079),#1254,.T.);
#12355=ADVANCED_FACE('',(#1643,#1080,#1081,#1082,#1083),#1255,.F.);
#12356=ADVANCED_FACE('',(#1644),#12020,.F.);
#12357=ADVANCED_FACE('',(#1645),#12021,.F.);
#12358=ADVANCED_FACE('',(#1646),#12022,.F.);
#12359=ADVANCED_FACE('',(#1647),#12023,.F.);
#12360=ADVANCED_FACE('',(#1648,#1084),#1256,.T.);
#12361=ADVANCED_FACE('',(#1649),#12024,.F.);
#12362=ADVANCED_FACE('',(#1650),#12025,.F.);
#12363=ADVANCED_FACE('',(#1651),#1257,.F.);
#12364=ADVANCED_FACE('',(#1652),#12026,.F.);
#12365=ADVANCED_FACE('',(#1653),#1258,.F.);
#12366=ADVANCED_FACE('',(#1654),#1259,.T.);
#12367=ADVANCED_FACE('',(#1655,#1085,#1086,#1087,#1088),#1260,.T.);
#12368=ADVANCED_FACE('',(#1656),#1261,.T.);
#12369=ADVANCED_FACE('',(#1657,#1089,#1090,#1091,#1092),#1262,.T.);
#12370=ADVANCED_FACE('',(#1658),#1263,.T.);
#12371=ADVANCED_FACE('',(#1659,#1093,#1094),#1264,.F.);
#12372=ADVANCED_FACE('',(#1660),#1265,.F.);
#12373=ADVANCED_FACE('',(#1661,#1095,#1096,#1097,#1098),#1266,.F.);
#12374=ADVANCED_FACE('',(#1662),#12027,.T.);
#12375=ADVANCED_FACE('',(#1663),#12028,.F.);
#12376=ADVANCED_FACE('',(#1664),#12029,.F.);
#12377=ADVANCED_FACE('',(#1665),#12030,.F.);
#12378=ADVANCED_FACE('',(#1666),#12031,.T.);
#12379=ADVANCED_FACE('',(#1667,#1099),#1267,.F.);
#12380=ADVANCED_FACE('',(#1668),#12032,.F.);
#12381=ADVANCED_FACE('',(#1669,#1100,#1101,#1102,#1103),#1268,.T.);
#12382=ADVANCED_FACE('',(#1670,#1104),#1269,.T.);
#12383=ADVANCED_FACE('',(#1671),#12033,.F.);
#12384=ADVANCED_FACE('',(#1672,#1105),#1270,.T.);
#12385=ADVANCED_FACE('',(#1673),#12034,.F.);
#12386=ADVANCED_FACE('',(#1674),#1271,.F.);
#12387=ADVANCED_FACE('',(#1675),#1272,.F.);
#12388=ADVANCED_FACE('',(#1676),#12035,.F.);
#12389=ADVANCED_FACE('',(#1677),#12036,.F.);
#12390=ADVANCED_FACE('',(#1678),#1273,.F.);
#12391=ADVANCED_FACE('',(#1679),#1274,.T.);
#12392=ADVANCED_FACE('',(#1680,#1106),#1275,.F.);
#12393=ADVANCED_FACE('',(#1681),#1276,.T.);
#12394=ADVANCED_FACE('',(#1682),#1277,.T.);
#12395=ADVANCED_FACE('',(#1683),#1278,.T.);
#12396=ADVANCED_FACE('',(#1684,#1107,#1108),#1279,.T.);
#12397=ADVANCED_FACE('',(#1685,#1109),#1280,.F.);
#12398=ADVANCED_FACE('',(#1686,#1110),#1281,.T.);
#12399=ADVANCED_FACE('',(#1687),#12037,.F.);
#12400=ADVANCED_FACE('',(#1688,#1111),#1282,.T.);
#12401=ADVANCED_FACE('',(#1689),#12038,.F.);
#12402=ADVANCED_FACE('',(#1690),#1283,.F.);
#12403=ADVANCED_FACE('',(#1691),#1284,.F.);
#12404=ADVANCED_FACE('',(#1692),#12039,.F.);
#12405=ADVANCED_FACE('',(#1693),#12040,.F.);
#12406=ADVANCED_FACE('',(#1694),#1285,.F.);
#12407=ADVANCED_FACE('',(#1695),#1286,.T.);
#12408=ADVANCED_FACE('',(#1696,#1112),#1287,.F.);
#12409=ADVANCED_FACE('',(#1697),#1288,.T.);
#12410=ADVANCED_FACE('',(#1698),#1289,.T.);
#12411=ADVANCED_FACE('',(#1699),#1290,.T.);
#12412=ADVANCED_FACE('',(#1700,#1113,#1114),#1291,.T.);
#12413=ADVANCED_FACE('',(#1701,#1115),#1292,.F.);
#12414=ADVANCED_FACE('',(#1702),#12041,.F.);
#12415=ADVANCED_FACE('',(#1703,#1116),#1293,.T.);
#12416=ADVANCED_FACE('',(#1704),#12042,.F.);
#12417=ADVANCED_FACE('',(#1705,#1117),#1294,.T.);
#12418=ADVANCED_FACE('',(#1706),#12043,.F.);
#12419=ADVANCED_FACE('',(#1707,#1118),#1295,.T.);
#12420=ADVANCED_FACE('',(#1708),#12044,.F.);
#12421=ADVANCED_FACE('',(#1709,#1119),#1296,.T.);
#12422=ADVANCED_FACE('',(#1710),#12045,.F.);
#12423=ADVANCED_FACE('',(#1711),#12046,.F.);
#12424=ADVANCED_FACE('',(#1712),#12047,.F.);
#12425=ADVANCED_FACE('',(#1713),#12048,.F.);
#12426=ADVANCED_FACE('',(#1714),#1297,.T.);
#12427=ADVANCED_FACE('',(#1715),#1298,.T.);
#12428=ADVANCED_FACE('',(#1716),#1299,.T.);
#12429=ADVANCED_FACE('',(#1717),#1300,.T.);
#12430=ADVANCED_FACE('',(#1718,#1120,#1121,#1122,#1123),#1301,.T.);
#12431=ADVANCED_FACE('',(#1719),#1302,.T.);
#12432=ADVANCED_FACE('',(#1720),#1303,.T.);
#12433=ADVANCED_FACE('',(#1721),#1304,.T.);
#12434=ADVANCED_FACE('',(#1722),#1305,.T.);
#12435=ADVANCED_FACE('',(#1723),#1306,.T.);
#12436=ADVANCED_FACE('',(#1724,#1124,#1125,#1126,#1127),#1307,.T.);
#12437=ADVANCED_FACE('',(#1725),#1308,.T.);
#12438=ADVANCED_FACE('',(#1726),#1309,.T.);
#12439=ADVANCED_FACE('',(#1727),#1310,.F.);
#12440=ADVANCED_FACE('',(#1728),#807,.F.);
#12441=ADVANCED_FACE('',(#1729),#12049,.T.);
#12442=ADVANCED_FACE('',(#1730),#12050,.F.);
#12443=ADVANCED_FACE('',(#1731),#777,.F.);
#12444=ADVANCED_FACE('',(#1732,#1128),#1311,.T.);
#12445=ADVANCED_FACE('',(#1733),#12051,.T.);
#12446=ADVANCED_FACE('',(#1734,#1129),#1312,.T.);
#12447=ADVANCED_FACE('',(#1735),#778,.F.);
#12448=ADVANCED_FACE('',(#1736),#808,.F.);
#12449=ADVANCED_FACE('',(#1737),#12052,.F.);
#12450=ADVANCED_FACE('',(#1738,#1130),#1313,.T.);
#12451=ADVANCED_FACE('',(#1739),#779,.T.);
#12452=ADVANCED_FACE('',(#1740),#12053,.T.);
#12453=ADVANCED_FACE('',(#1741),#780,.T.);
#12454=ADVANCED_FACE('',(#1742,#1131),#1314,.T.);
#12455=ADVANCED_FACE('',(#1743),#12054,.F.);
#12456=ADVANCED_FACE('',(#1744),#747,.T.);
#12457=ADVANCED_FACE('',(#1745),#748,.T.);
#12458=ADVANCED_FACE('',(#1746),#749,.T.);
#12459=ADVANCED_FACE('',(#1747),#750,.T.);
#12460=ADVANCED_FACE('',(#1748),#751,.T.);
#12461=ADVANCED_FACE('',(#1749),#752,.T.);
#12462=ADVANCED_FACE('',(#1750),#753,.T.);
#12463=ADVANCED_FACE('',(#1751),#754,.F.);
#12464=ADVANCED_FACE('',(#1752),#12055,.T.);
#12465=ADVANCED_FACE('',(#1753),#1315,.T.);
#12466=ADVANCED_FACE('',(#1754),#755,.F.);
#12467=ADVANCED_FACE('',(#1755),#1316,.T.);
#12468=ADVANCED_FACE('',(#1756),#756,.F.);
#12469=ADVANCED_FACE('',(#1757),#1317,.T.);
#12470=ADVANCED_FACE('',(#1758),#757,.F.);
#12471=ADVANCED_FACE('',(#1759),#1318,.T.);
#12472=ADVANCED_FACE('',(#1760),#758,.F.);
#12473=ADVANCED_FACE('',(#1761),#1319,.T.);
#12474=ADVANCED_FACE('',(#1762),#759,.F.);
#12475=ADVANCED_FACE('',(#1763),#12056,.F.);
#12476=ADVANCED_FACE('',(#1764),#1320,.T.);
#12477=ADVANCED_FACE('',(#1765),#760,.F.);
#12478=ADVANCED_FACE('',(#1766,#1132),#1321,.T.);
#12479=ADVANCED_FACE('',(#1767),#1322,.T.);
#12480=ADVANCED_FACE('',(#1768,#1133),#1323,.T.);
#12481=ADVANCED_FACE('',(#1769),#12057,.T.);
#12482=ADVANCED_FACE('',(#1770,#1134),#1324,.T.);
#12483=ADVANCED_FACE('',(#1771),#12058,.F.);
#12484=ADVANCED_FACE('',(#1772,#1135),#1325,.T.);
#12485=ADVANCED_FACE('',(#1773),#12059,.T.);
#12486=ADVANCED_FACE('',(#1774,#1136),#1326,.T.);
#12487=ADVANCED_FACE('',(#1775),#12060,.F.);
#12488=ADVANCED_FACE('',(#1776),#809,.F.);
#12489=ADVANCED_FACE('',(#1777),#12061,.T.);
#12490=ADVANCED_FACE('',(#1778),#12062,.F.);
#12491=ADVANCED_FACE('',(#1779),#781,.F.);
#12492=ADVANCED_FACE('',(#1780,#1137),#1327,.T.);
#12493=ADVANCED_FACE('',(#1781),#12063,.T.);
#12494=ADVANCED_FACE('',(#1782,#1138),#1328,.T.);
#12495=ADVANCED_FACE('',(#1783),#782,.F.);
#12496=ADVANCED_FACE('',(#1784),#810,.F.);
#12497=ADVANCED_FACE('',(#1785),#12064,.F.);
#12498=ADVANCED_FACE('',(#1786,#1139),#1329,.T.);
#12499=ADVANCED_FACE('',(#1787),#783,.T.);
#12500=ADVANCED_FACE('',(#1788),#12065,.T.);
#12501=ADVANCED_FACE('',(#1789),#784,.T.);
#12502=ADVANCED_FACE('',(#1790,#1140),#1330,.T.);
#12503=ADVANCED_FACE('',(#1791),#12066,.F.);
#12504=ADVANCED_FACE('',(#1792),#761,.T.);
#12505=ADVANCED_FACE('',(#1793),#762,.T.);
#12506=ADVANCED_FACE('',(#1794),#763,.T.);
#12507=ADVANCED_FACE('',(#1795),#764,.T.);
#12508=ADVANCED_FACE('',(#1796),#765,.T.);
#12509=ADVANCED_FACE('',(#1797),#766,.T.);
#12510=ADVANCED_FACE('',(#1798),#767,.T.);
#12511=ADVANCED_FACE('',(#1799),#768,.T.);
#12512=ADVANCED_FACE('',(#1800),#769,.F.);
#12513=ADVANCED_FACE('',(#1801),#12067,.T.);
#12514=ADVANCED_FACE('',(#1802),#1331,.T.);
#12515=ADVANCED_FACE('',(#1803),#770,.F.);
#12516=ADVANCED_FACE('',(#1804),#1332,.T.);
#12517=ADVANCED_FACE('',(#1805),#771,.F.);
#12518=ADVANCED_FACE('',(#1806),#1333,.T.);
#12519=ADVANCED_FACE('',(#1807),#772,.F.);
#12520=ADVANCED_FACE('',(#1808),#1334,.T.);
#12521=ADVANCED_FACE('',(#1809),#773,.F.);
#12522=ADVANCED_FACE('',(#1810),#1335,.T.);
#12523=ADVANCED_FACE('',(#1811),#774,.F.);
#12524=ADVANCED_FACE('',(#1812),#1336,.T.);
#12525=ADVANCED_FACE('',(#1813),#775,.F.);
#12526=ADVANCED_FACE('',(#1814),#12068,.F.);
#12527=ADVANCED_FACE('',(#1815),#1337,.T.);
#12528=ADVANCED_FACE('',(#1816),#776,.F.);
#12529=ADVANCED_FACE('',(#1817,#1141),#1338,.T.);
#12530=ADVANCED_FACE('',(#1818),#1339,.T.);
#12531=ADVANCED_FACE('',(#1819,#1142),#1340,.T.);
#12532=ADVANCED_FACE('',(#1820),#12069,.T.);
#12533=ADVANCED_FACE('',(#1821,#1143),#1341,.T.);
#12534=ADVANCED_FACE('',(#1822),#12070,.F.);
#12535=ADVANCED_FACE('',(#1823,#1144),#1342,.T.);
#12536=ADVANCED_FACE('',(#1824),#12071,.T.);
#12537=ADVANCED_FACE('',(#1825,#1145),#1343,.T.);
#12538=ADVANCED_FACE('',(#1826),#12072,.F.);
#12539=ADVANCED_FACE('',(#1827),#1344,.F.);
#12540=ADVANCED_FACE('',(#1828),#1345,.F.);
#12541=ADVANCED_FACE('',(#1829),#1346,.F.);
#12542=ADVANCED_FACE('',(#1830),#1347,.F.);
#12543=ADVANCED_FACE('',(#1831),#1348,.F.);
#12544=ADVANCED_FACE('',(#1832),#1349,.F.);
#12545=ADVANCED_FACE('',(#1833),#1350,.F.);
#12546=ADVANCED_FACE('',(#1834),#1351,.F.);
#12547=ADVANCED_FACE('',(#1835),#1352,.F.);
#12548=ADVANCED_FACE('',(#1836),#1353,.F.);
#12549=ADVANCED_FACE('',(#1837),#1354,.F.);
#12550=ADVANCED_FACE('',(#1838),#1355,.F.);
#12551=ADVANCED_FACE('',(#1839),#1356,.F.);
#12552=ADVANCED_FACE('',(#1840),#1357,.F.);
#12553=ADVANCED_FACE('',(#1841),#1358,.F.);
#12554=ADVANCED_FACE('',(#1842),#1359,.F.);
#12555=ADVANCED_FACE('',(#1843),#1360,.F.);
#12556=ADVANCED_FACE('',(#1844),#1361,.F.);
#12557=ADVANCED_FACE('',(#1845),#1362,.F.);
#12558=ADVANCED_FACE('',(#1846),#1363,.F.);
#12559=ADVANCED_FACE('',(#1847),#1364,.F.);
#12560=ADVANCED_FACE('',(#1848),#1365,.F.);
#12561=ADVANCED_FACE('',(#1849),#1366,.F.);
#12562=ADVANCED_FACE('',(#1850),#1367,.F.);
#12563=ADVANCED_FACE('',(#1851),#1368,.F.);
#12564=ADVANCED_FACE('',(#1852),#1369,.F.);
#12565=ADVANCED_FACE('',(#1853),#1370,.F.);
#12566=ADVANCED_FACE('',(#1854),#1371,.F.);
#12567=ADVANCED_FACE('',(#1855),#1372,.F.);
#12568=ADVANCED_FACE('',(#1856),#1373,.F.);
#12569=ADVANCED_FACE('',(#1857),#1374,.F.);
#12570=ADVANCED_FACE('',(#1858),#1375,.F.);
#12571=ADVANCED_FACE('',(#1859),#1376,.F.);
#12572=ADVANCED_FACE('',(#1860),#1377,.F.);
#12573=ADVANCED_FACE('',(#1861),#1378,.F.);
#12574=ADVANCED_FACE('',(#1862),#1379,.F.);
#12575=ADVANCED_FACE('',(#1863),#12073,.F.);
#12576=ADVANCED_FACE('',(#1864),#1380,.T.);
#12577=ADVANCED_FACE('',(#1865),#1381,.T.);
#12578=ADVANCED_FACE('',(#1866),#1382,.T.);
#12579=ADVANCED_FACE('',(#1867),#1383,.T.);
#12580=ADVANCED_FACE('',(#1868),#1384,.T.);
#12581=ADVANCED_FACE('',(#1869),#1385,.T.);
#12582=ADVANCED_FACE('',(#1870),#1386,.T.);
#12583=ADVANCED_FACE('',(#1871),#1387,.T.);
#12584=ADVANCED_FACE('',(#1872,#1146),#1388,.T.);
#12585=ADVANCED_FACE('',(#1873,#1147),#1389,.F.);
#12586=ADVANCED_FACE('',(#1874),#1390,.T.);
#12587=ADVANCED_FACE('',(#1875),#12074,.F.);
#12588=ADVANCED_FACE('',(#1876),#1391,.F.);
#12589=ADVANCED_FACE('',(#1877),#1392,.F.);
#12590=ADVANCED_FACE('',(#1878),#1393,.T.);
#12591=ADVANCED_FACE('',(#1879),#1394,.T.);
#12592=ADVANCED_FACE('',(#1880),#1395,.T.);
#12593=ADVANCED_FACE('',(#1881),#1396,.T.);
#12594=ADVANCED_FACE('',(#1882),#1397,.T.);
#12595=ADVANCED_FACE('',(#1883,#1148),#1398,.T.);
#12596=ADVANCED_FACE('',(#1884),#785,.F.);
#12597=ADVANCED_FACE('',(#1885),#12075,.F.);
#12598=ADVANCED_FACE('',(#1886,#1149),#1399,.T.);
#12599=ADVANCED_FACE('',(#1887),#12076,.T.);
#12600=ADVANCED_FACE('',(#1888,#1150),#1400,.F.);
#12601=ADVANCED_FACE('',(#1889),#1401,.F.);
#12602=ADVANCED_FACE('',(#1890),#1402,.F.);
#12603=ADVANCED_FACE('',(#1891),#1403,.F.);
#12604=ADVANCED_FACE('',(#1892),#1404,.F.);
#12605=ADVANCED_FACE('',(#1893),#1405,.F.);
#12606=ADVANCED_FACE('',(#1894),#1406,.F.);
#12607=ADVANCED_FACE('',(#1895),#1407,.F.);
#12608=ADVANCED_FACE('',(#1896),#1408,.F.);
#12609=ADVANCED_FACE('',(#1897),#1409,.F.);
#12610=ADVANCED_FACE('',(#1898),#1410,.T.);
#12611=ADVANCED_FACE('',(#1899),#786,.T.);
#12612=ADVANCED_FACE('',(#1900),#12077,.T.);
#12613=ADVANCED_FACE('',(#1901),#787,.T.);
#12614=ADVANCED_FACE('',(#1902,#1151),#1411,.T.);
#12615=ADVANCED_FACE('',(#1903),#788,.T.);
#12616=ADVANCED_FACE('',(#1904),#12078,.T.);
#12617=ADVANCED_FACE('',(#1905),#12079,.F.);
#12618=ADVANCED_FACE('',(#1906),#12080,.F.);
#12619=ADVANCED_FACE('',(#1907),#12081,.F.);
#12620=ADVANCED_FACE('',(#1908),#12082,.F.);
#12621=ADVANCED_FACE('',(#1909),#1412,.T.);
#12622=ADVANCED_FACE('',(#1910),#1413,.T.);
#12623=ADVANCED_FACE('',(#1911),#1414,.T.);
#12624=ADVANCED_FACE('',(#1912),#1415,.T.);
#12625=ADVANCED_FACE('',(#1913,#1152,#1153,#1154,#1155),#1416,.T.);
#12626=ADVANCED_FACE('',(#1914,#1156,#1157,#1158,#1159),#1417,.F.);
#12627=ADVANCED_FACE('',(#1915),#12083,.F.);
#12628=ADVANCED_FACE('',(#1916),#12084,.F.);
#12629=ADVANCED_FACE('',(#1917),#12085,.F.);
#12630=ADVANCED_FACE('',(#1918),#12086,.F.);
#12631=ADVANCED_FACE('',(#1919),#12087,.F.);
#12632=ADVANCED_FACE('',(#1920),#12088,.F.);
#12633=ADVANCED_FACE('',(#1921),#12089,.F.);
#12634=ADVANCED_FACE('',(#1922),#12090,.F.);
#12635=ADVANCED_FACE('',(#1923),#1418,.T.);
#12636=ADVANCED_FACE('',(#1924),#1419,.T.);
#12637=ADVANCED_FACE('',(#1925),#1420,.T.);
#12638=ADVANCED_FACE('',(#1926),#1421,.T.);
#12639=ADVANCED_FACE('',(#1927,#1160,#1161,#1162,#1163,#1164,#1165,#1166,
#1167),#1422,.T.);
#12640=ADVANCED_FACE('',(#1928,#1168,#1169,#1170,#1171,#1172,#1173,#1174,
#1175),#1423,.F.);
#12641=ADVANCED_FACE('',(#1929),#12091,.F.);
#12642=ADVANCED_FACE('',(#1930),#1424,.T.);
#12643=ADVANCED_FACE('',(#1931),#12092,.F.);
#12644=ADVANCED_FACE('',(#1932),#1425,.T.);
#12645=ADVANCED_FACE('',(#1933),#12093,.F.);
#12646=ADVANCED_FACE('',(#1934),#1426,.T.);
#12647=ADVANCED_FACE('',(#1935),#12094,.F.);
#12648=ADVANCED_FACE('',(#1936),#1427,.T.);
#12649=ADVANCED_FACE('',(#1937),#12095,.F.);
#12650=ADVANCED_FACE('',(#1938),#1428,.T.);
#12651=ADVANCED_FACE('',(#1939),#12096,.F.);
#12652=ADVANCED_FACE('',(#1940),#1429,.T.);
#12653=ADVANCED_FACE('',(#1941),#12097,.F.);
#12654=ADVANCED_FACE('',(#1942),#1430,.T.);
#12655=ADVANCED_FACE('',(#1943),#12098,.F.);
#12656=ADVANCED_FACE('',(#1944),#1431,.T.);
#12657=ADVANCED_FACE('',(#1945,#1176,#1177,#1178,#1179),#1432,.T.);
#12658=ADVANCED_FACE('',(#1946),#1433,.T.);
#12659=ADVANCED_FACE('',(#1947,#1180),#1434,.T.);
#12660=ADVANCED_FACE('',(#1948,#1181,#1182,#1183,#1184),#1435,.T.);
#12661=ADVANCED_FACE('',(#1949),#1436,.F.);
#12662=ADVANCED_FACE('',(#1950),#1437,.T.);
#12663=ADVANCED_FACE('',(#1951),#12099,.F.);
#12664=ADVANCED_FACE('',(#1952),#1438,.T.);
#12665=ADVANCED_FACE('',(#1953),#12100,.F.);
#12666=ADVANCED_FACE('',(#1954),#1439,.T.);
#12667=ADVANCED_FACE('',(#1955),#12101,.F.);
#12668=ADVANCED_FACE('',(#1956),#1440,.T.);
#12669=ADVANCED_FACE('',(#1957),#12102,.F.);
#12670=ADVANCED_FACE('',(#1958),#1441,.T.);
#12671=ADVANCED_FACE('',(#1959),#1442,.T.);
#12672=ADVANCED_FACE('',(#1960),#1443,.T.);
#12673=ADVANCED_FACE('',(#1961),#1444,.T.);
#12674=ADVANCED_FACE('',(#1962),#1445,.T.);
#12675=ADVANCED_FACE('',(#1963,#1185,#1186,#1187,#1188),#1446,.T.);
#12676=ADVANCED_FACE('',(#1964),#1447,.T.);
#12677=ADVANCED_FACE('',(#1965),#1448,.T.);
#12678=ADVANCED_FACE('',(#1966),#1449,.T.);
#12679=ADVANCED_FACE('',(#1967),#1450,.T.);
#12680=ADVANCED_FACE('',(#1968),#1451,.T.);
#12681=ADVANCED_FACE('',(#1969),#1452,.T.);
#12682=ADVANCED_FACE('',(#1970),#1453,.T.);
#12683=ADVANCED_FACE('',(#1971),#1454,.T.);
#12684=ADVANCED_FACE('',(#1972),#1455,.T.);
#12685=ADVANCED_FACE('',(#1973),#1456,.T.);
#12686=ADVANCED_FACE('',(#1974),#1457,.T.);
#12687=ADVANCED_FACE('',(#1975),#1458,.T.);
#12688=ADVANCED_FACE('',(#1976),#1459,.T.);
#12689=ADVANCED_FACE('',(#1977),#1460,.T.);
#12690=ADVANCED_FACE('',(#1978),#1461,.T.);
#12691=ADVANCED_FACE('',(#1979),#1462,.T.);
#12692=ADVANCED_FACE('',(#1980),#1463,.T.);
#12693=ADVANCED_FACE('',(#1981),#1464,.F.);
#12694=ADVANCED_FACE('',(#1982),#1465,.T.);
#12695=ADVANCED_FACE('',(#1983),#1466,.T.);
#12696=ADVANCED_FACE('',(#1984),#1467,.T.);
#12697=ADVANCED_FACE('',(#1985),#1468,.T.);
#12698=ADVANCED_FACE('',(#1986),#1469,.T.);
#12699=ADVANCED_FACE('',(#1987),#1470,.T.);
#12700=ADVANCED_FACE('',(#1988),#1471,.T.);
#12701=ADVANCED_FACE('',(#1989),#1472,.T.);
#12702=ADVANCED_FACE('',(#1990),#1473,.T.);
#12703=ADVANCED_FACE('',(#1991),#1474,.T.);
#12704=ADVANCED_FACE('',(#1992),#789,.F.);
#12705=ADVANCED_FACE('',(#1993),#12103,.F.);
#12706=ADVANCED_FACE('',(#1994,#1189),#1475,.T.);
#12707=ADVANCED_FACE('',(#1995),#12104,.T.);
#12708=ADVANCED_FACE('',(#1996,#1190),#1476,.F.);
#12709=ADVANCED_FACE('',(#1997),#1477,.F.);
#12710=ADVANCED_FACE('',(#1998),#1478,.F.);
#12711=ADVANCED_FACE('',(#1999),#1479,.F.);
#12712=ADVANCED_FACE('',(#2000),#1480,.F.);
#12713=ADVANCED_FACE('',(#2001),#1481,.F.);
#12714=ADVANCED_FACE('',(#2002),#1482,.F.);
#12715=ADVANCED_FACE('',(#2003),#1483,.F.);
#12716=ADVANCED_FACE('',(#2004),#1484,.F.);
#12717=ADVANCED_FACE('',(#2005,#1191),#1485,.T.);
#12718=ADVANCED_FACE('',(#2006),#12105,.T.);
#12719=ADVANCED_FACE('',(#2007),#1486,.F.);
#12720=ADVANCED_FACE('',(#2008),#1487,.T.);
#12721=ADVANCED_FACE('',(#2009),#790,.T.);
#12722=ADVANCED_FACE('',(#2010),#12106,.T.);
#12723=ADVANCED_FACE('',(#2011),#791,.T.);
#12724=ADVANCED_FACE('',(#2012,#1192),#1488,.T.);
#12725=ADVANCED_FACE('',(#2013),#792,.T.);
#12726=ADVANCED_FACE('',(#2014),#12107,.T.);
#12727=ADVANCED_FACE('',(#2015),#12108,.F.);
#12728=ADVANCED_FACE('',(#2016),#12109,.F.);
#12729=ADVANCED_FACE('',(#2017),#12110,.F.);
#12730=ADVANCED_FACE('',(#2018),#12111,.F.);
#12731=ADVANCED_FACE('',(#2019),#12112,.F.);
#12732=ADVANCED_FACE('',(#2020),#12113,.F.);
#12733=ADVANCED_FACE('',(#2021),#12114,.F.);
#12734=ADVANCED_FACE('',(#2022),#12115,.F.);
#12735=ADVANCED_FACE('',(#2023),#12116,.F.);
#12736=ADVANCED_FACE('',(#2024),#12117,.F.);
#12737=ADVANCED_FACE('',(#2025),#12118,.F.);
#12738=ADVANCED_FACE('',(#2026),#12119,.F.);
#12739=ADVANCED_FACE('',(#2027),#12120,.F.);
#12740=ADVANCED_FACE('',(#2028),#12121,.F.);
#12741=ADVANCED_FACE('',(#2029),#12122,.F.);
#12742=ADVANCED_FACE('',(#2030),#12123,.F.);
#12743=ADVANCED_FACE('',(#2031),#12124,.F.);
#12744=ADVANCED_FACE('',(#2032),#12125,.F.);
#12745=ADVANCED_FACE('',(#2033),#12126,.F.);
#12746=ADVANCED_FACE('',(#2034),#11,.F.);
#12747=ADVANCED_FACE('',(#2035),#12,.F.);
#12748=ADVANCED_FACE('',(#2036,#1193,#1194,#1195,#1196),#1489,.T.);
#12749=ADVANCED_FACE('',(#2037),#12127,.F.);
#12750=ADVANCED_FACE('',(#2038),#12128,.F.);
#12751=ADVANCED_FACE('',(#2039),#12129,.F.);
#12752=ADVANCED_FACE('',(#2040),#1490,.F.);
#12753=ADVANCED_FACE('',(#2041,#1197,#1198,#1199,#1200),#1491,.F.);
#12754=ADVANCED_FACE('',(#2042),#12130,.T.);
#12755=ADVANCED_FACE('',(#2043),#12131,.F.);
#12756=ADVANCED_FACE('',(#2044),#12132,.T.);
#12757=ADVANCED_FACE('',(#2045,#1201),#1492,.F.);
#12758=ADVANCED_FACE('',(#2046),#1493,.T.);
#12759=ADVANCED_FACE('',(#2047),#793,.T.);
#12760=ADVANCED_FACE('',(#2048),#12133,.T.);
#12761=ADVANCED_FACE('',(#2049),#794,.T.);
#12762=ADVANCED_FACE('',(#2050,#1202),#1494,.T.);
#12763=ADVANCED_FACE('',(#2051),#795,.T.);
#12764=ADVANCED_FACE('',(#2052),#12134,.T.);
#12765=ADVANCED_FACE('',(#2053),#796,.T.);
#12766=ADVANCED_FACE('',(#2054),#1495,.T.);
#12767=ADVANCED_FACE('',(#2055),#1496,.F.);
#12768=ADVANCED_FACE('',(#2056),#1497,.F.);
#12769=ADVANCED_FACE('',(#2057),#1498,.F.);
#12770=ADVANCED_FACE('',(#2058),#1499,.F.);
#12771=ADVANCED_FACE('',(#2059),#1500,.F.);
#12772=ADVANCED_FACE('',(#2060),#1501,.F.);
#12773=ADVANCED_FACE('',(#2061),#1502,.F.);
#12774=ADVANCED_FACE('',(#2062),#1503,.F.);
#12775=ADVANCED_FACE('',(#2063),#1504,.T.);
#12776=ADVANCED_FACE('',(#2064),#797,.T.);
#12777=ADVANCED_FACE('',(#2065),#12135,.T.);
#12778=ADVANCED_FACE('',(#2066),#798,.T.);
#12779=ADVANCED_FACE('',(#2067,#1203),#1505,.T.);
#12780=ADVANCED_FACE('',(#2068),#799,.T.);
#12781=ADVANCED_FACE('',(#2069),#12136,.T.);
#12782=ADVANCED_FACE('',(#2070),#800,.T.);
#12783=ADVANCED_FACE('',(#2071),#1506,.T.);
#12784=ADVANCED_FACE('',(#2072),#1507,.F.);
#12785=ADVANCED_FACE('',(#2073),#1508,.F.);
#12786=ADVANCED_FACE('',(#2074),#1509,.F.);
#12787=ADVANCED_FACE('',(#2075),#1510,.F.);
#12788=ADVANCED_FACE('',(#2076),#1511,.F.);
#12789=ADVANCED_FACE('',(#2077),#1512,.F.);
#12790=ADVANCED_FACE('',(#2078),#1513,.F.);
#12791=ADVANCED_FACE('',(#2079),#1514,.F.);
#12792=ADVANCED_FACE('',(#2080),#12137,.T.);
#12793=ADVANCED_FACE('',(#2081),#12138,.T.);
#12794=ADVANCED_FACE('',(#2082),#12139,.T.);
#12795=ADVANCED_FACE('',(#2083),#12140,.T.);
#12796=ADVANCED_FACE('',(#2084),#12141,.T.);
#12797=ADVANCED_FACE('',(#2085),#12142,.T.);
#12798=ADVANCED_FACE('',(#2086),#12143,.T.);
#12799=ADVANCED_FACE('',(#2087),#12144,.T.);
#12800=ADVANCED_FACE('',(#2088),#12145,.T.);
#12801=ADVANCED_FACE('',(#2089),#12146,.T.);
#12802=ADVANCED_FACE('',(#2090),#12147,.T.);
#12803=ADVANCED_FACE('',(#2091),#12148,.T.);
#12804=ADVANCED_FACE('',(#2092),#12149,.T.);
#12805=ADVANCED_FACE('',(#2093),#12150,.T.);
#12806=ADVANCED_FACE('',(#2094),#12151,.T.);
#12807=ADVANCED_FACE('',(#2095),#12152,.T.);
#12808=ADVANCED_FACE('',(#2096),#12153,.T.);
#12809=ADVANCED_FACE('',(#2097),#12154,.T.);
#12810=ADVANCED_FACE('',(#2098),#12155,.T.);
#12811=ADVANCED_FACE('',(#2099),#12156,.T.);
#12812=ADVANCED_FACE('',(#2100),#12157,.T.);
#12813=ADVANCED_FACE('',(#2101),#12158,.T.);
#12814=ADVANCED_FACE('',(#2102),#12159,.T.);
#12815=ADVANCED_FACE('',(#2103),#12160,.T.);
#12816=ADVANCED_FACE('',(#2104),#12161,.T.);
#12817=ADVANCED_FACE('',(#2105),#12162,.T.);
#12818=ADVANCED_FACE('',(#2106),#12163,.T.);
#12819=ADVANCED_FACE('',(#2107),#12164,.T.);
#12820=ADVANCED_FACE('',(#2108),#12165,.T.);
#12821=ADVANCED_FACE('',(#2109),#12166,.T.);
#12822=ADVANCED_FACE('',(#2110),#12167,.T.);
#12823=ADVANCED_FACE('',(#2111),#12168,.T.);
#12824=ADVANCED_FACE('',(#2112),#12169,.T.);
#12825=ADVANCED_FACE('',(#2113),#12170,.T.);
#12826=ADVANCED_FACE('',(#2114),#12171,.T.);
#12827=ADVANCED_FACE('',(#2115),#12172,.T.);
#12828=ADVANCED_FACE('',(#2116),#12173,.T.);
#12829=ADVANCED_FACE('',(#2117),#12174,.T.);
#12830=ADVANCED_FACE('',(#2118),#12175,.T.);
#12831=ADVANCED_FACE('',(#2119),#12176,.T.);
#12832=ADVANCED_FACE('',(#2120),#12177,.T.);
#12833=ADVANCED_FACE('',(#2121),#12178,.T.);
#12834=ADVANCED_FACE('',(#2122),#12179,.T.);
#12835=ADVANCED_FACE('',(#2123),#12180,.T.);
#12836=ADVANCED_FACE('',(#2124),#12181,.T.);
#12837=ADVANCED_FACE('',(#2125),#12182,.T.);
#12838=ADVANCED_FACE('',(#2126),#12183,.T.);
#12839=ADVANCED_FACE('',(#2127),#12184,.T.);
#12840=ADVANCED_FACE('',(#2128),#12185,.T.);
#12841=ADVANCED_FACE('',(#2129),#12186,.T.);
#12842=ADVANCED_FACE('',(#2130),#12187,.T.);
#12843=ADVANCED_FACE('',(#2131),#12188,.T.);
#12844=ADVANCED_FACE('',(#2132),#12189,.T.);
#12845=ADVANCED_FACE('',(#2133),#12190,.T.);
#12846=ADVANCED_FACE('',(#2134),#12191,.T.);
#12847=ADVANCED_FACE('',(#2135),#12192,.T.);
#12848=ADVANCED_FACE('',(#2136),#12193,.T.);
#12849=ADVANCED_FACE('',(#2137),#12194,.T.);
#12850=ADVANCED_FACE('',(#2138),#12195,.T.);
#12851=ADVANCED_FACE('',(#2139),#12196,.T.);
#12852=ADVANCED_FACE('',(#2140),#12197,.T.);
#12853=ADVANCED_FACE('',(#2141),#12198,.T.);
#12854=ADVANCED_FACE('',(#2142),#12199,.T.);
#12855=ADVANCED_FACE('',(#2143),#12200,.T.);
#12856=ADVANCED_FACE('',(#2144),#12201,.T.);
#12857=ADVANCED_FACE('',(#2145),#12202,.T.);
#12858=ADVANCED_FACE('',(#2146),#12203,.T.);
#12859=ADVANCED_FACE('',(#2147),#12204,.T.);
#12860=ADVANCED_FACE('',(#2148),#12205,.T.);
#12861=ADVANCED_FACE('',(#2149),#12206,.T.);
#12862=ADVANCED_FACE('',(#2150),#12207,.T.);
#12863=ADVANCED_FACE('',(#2151),#12208,.T.);
#12864=ADVANCED_FACE('',(#2152),#12209,.T.);
#12865=ADVANCED_FACE('',(#2153),#12210,.T.);
#12866=ADVANCED_FACE('',(#2154),#12211,.T.);
#12867=ADVANCED_FACE('',(#2155),#12212,.T.);
#12868=ADVANCED_FACE('',(#2156),#12213,.T.);
#12869=ADVANCED_FACE('',(#2157),#12214,.T.);
#12870=ADVANCED_FACE('',(#2158),#12215,.T.);
#12871=ADVANCED_FACE('',(#2159),#12216,.T.);
#12872=ADVANCED_FACE('',(#2160),#12217,.T.);
#12873=ADVANCED_FACE('',(#2161),#12218,.T.);
#12874=ADVANCED_FACE('',(#2162),#12219,.T.);
#12875=ADVANCED_FACE('',(#2163),#12220,.T.);
#12876=ADVANCED_FACE('',(#2164),#12221,.T.);
#12877=ADVANCED_FACE('',(#2165),#12222,.T.);
#12878=ADVANCED_FACE('',(#2166),#12223,.T.);
#12879=ADVANCED_FACE('',(#2167),#12224,.T.);
#12880=ADVANCED_FACE('',(#2168),#12225,.T.);
#12881=ADVANCED_FACE('',(#2169),#12226,.T.);
#12882=ADVANCED_FACE('',(#2170),#12227,.T.);
#12883=ADVANCED_FACE('',(#2171),#12228,.T.);
#12884=ADVANCED_FACE('',(#2172),#12229,.T.);
#12885=ADVANCED_FACE('',(#2173),#12230,.T.);
#12886=ADVANCED_FACE('',(#2174),#12231,.T.);
#12887=ADVANCED_FACE('',(#2175),#12232,.T.);
#12888=ADVANCED_FACE('',(#2176),#12233,.T.);
#12889=ADVANCED_FACE('',(#2177),#12234,.T.);
#12890=ADVANCED_FACE('',(#2178),#12235,.T.);
#12891=ADVANCED_FACE('',(#2179),#12236,.T.);
#12892=ADVANCED_FACE('',(#2180),#12237,.T.);
#12893=ADVANCED_FACE('',(#2181),#12238,.T.);
#12894=ADVANCED_FACE('',(#2182),#12239,.T.);
#12895=ADVANCED_FACE('',(#2183),#12240,.T.);
#12896=ADVANCED_FACE('',(#2184),#12241,.T.);
#12897=ADVANCED_FACE('',(#2185),#12242,.T.);
#12898=ADVANCED_FACE('',(#2186),#12243,.T.);
#12899=ADVANCED_FACE('',(#2187),#12244,.T.);
#12900=ADVANCED_FACE('',(#2188),#12245,.T.);
#12901=ADVANCED_FACE('',(#2189),#12246,.T.);
#12902=ADVANCED_FACE('',(#2190),#12247,.T.);
#12903=ADVANCED_FACE('',(#2191),#12248,.T.);
#12904=ADVANCED_FACE('',(#2192),#12249,.T.);
#12905=ADVANCED_FACE('',(#2193),#12250,.T.);
#12906=ADVANCED_FACE('',(#2194),#12251,.T.);
#12907=ADVANCED_FACE('',(#2195),#12252,.T.);
#12908=ADVANCED_FACE('',(#2196),#12253,.T.);
#12909=ADVANCED_FACE('',(#2197),#12254,.T.);
#12910=ADVANCED_FACE('',(#2198),#12255,.T.);
#12911=ADVANCED_FACE('',(#2199),#12256,.T.);
#12912=ADVANCED_FACE('',(#2200),#12257,.T.);
#12913=ADVANCED_FACE('',(#2201),#12258,.T.);
#12914=ADVANCED_FACE('',(#2202),#12259,.T.);
#12915=ADVANCED_FACE('',(#2203),#12260,.T.);
#12916=ADVANCED_FACE('',(#2204),#12261,.T.);
#12917=ADVANCED_FACE('',(#2205),#12262,.T.);
#12918=ADVANCED_FACE('',(#2206,#1204),#1515,.T.);
#12919=ADVANCED_FACE('',(#2207),#12263,.T.);
#12920=ADVANCED_FACE('',(#2208),#1516,.F.);
#12921=ADVANCED_FACE('',(#2209),#13,.F.);
#12922=ADVANCED_FACE('',(#2210),#12264,.T.);
#12923=ADVANCED_FACE('',(#2211),#14,.F.);
#12924=ADVANCED_FACE('',(#2212),#1517,.F.);
#12925=ADVANCED_FACE('',(#2213),#1518,.T.);
#12926=ADVANCED_FACE('',(#2214),#1519,.F.);
#12927=ADVANCED_FACE('',(#2215),#1520,.F.);
#12928=ADVANCED_FACE('',(#2216),#1521,.F.);
#12929=ADVANCED_FACE('',(#2217,#1205),#12265,.T.);
#12930=ADVANCED_FACE('',(#2218),#1522,.T.);
#12931=ADVANCED_FACE('',(#2219,#1206),#1523,.F.);
#12932=ADVANCED_FACE('',(#2220),#12266,.T.);
#12933=ADVANCED_FACE('',(#2221,#1207),#1524,.T.);
#12934=ADVANCED_FACE('',(#2222),#12267,.T.);
#12935=ADVANCED_FACE('',(#2223),#12268,.F.);
#12936=ADVANCED_FACE('',(#2224),#12269,.T.);
#12937=ADVANCED_FACE('',(#2225,#1208),#1525,.T.);
#12938=ADVANCED_FACE('',(#2226,#1209),#1526,.F.);
#12939=ADVANCED_FACE('',(#2227),#1527,.T.);
#12940=ADVANCED_FACE('',(#2228),#12270,.F.);
#12941=ADVANCED_FACE('',(#2229),#1528,.T.);
#12942=ADVANCED_FACE('',(#2230,#1210),#12271,.F.);
#12943=ADVANCED_FACE('',(#2231,#1211),#12272,.T.);
#12944=ADVANCED_FACE('',(#2232,#1212),#1529,.T.);
#12945=ADVANCED_FACE('',(#2233,#1213),#1530,.F.);
#12946=ADVANCED_FACE('',(#2234),#12273,.F.);
#12947=ADVANCED_FACE('',(#2235),#1531,.T.);
#12948=ADVANCED_FACE('',(#2236),#12274,.F.);
#12949=ADVANCED_FACE('',(#2237),#1532,.T.);
#12950=ADVANCED_FACE('',(#2238),#1533,.F.);
#12951=ADVANCED_FACE('',(#2239),#1534,.F.);
#12952=ADVANCED_FACE('',(#2240),#1535,.F.);
#12953=ADVANCED_FACE('',(#2241,#1214,#1215),#1536,.T.);
#12954=ADVANCED_FACE('',(#2242,#1216,#1217),#1537,.F.);
#12955=ADVANCED_FACE('',(#2243),#12275,.T.);
#12956=ADVANCED_FACE('',(#2244,#1218),#12276,.F.);
#12957=ADVANCED_FACE('',(#2245,#1219),#12277,.T.);
#12958=ADVANCED_FACE('',(#2246),#1538,.F.);
#12959=ADVANCED_FACE('',(#2247),#12278,.F.);
#12960=ADVANCED_FACE('',(#2248),#12279,.T.);
#12961=ADVANCED_FACE('',(#2249,#1220),#1539,.T.);
#12962=ADVANCED_FACE('',(#2250,#1221),#1540,.F.);
#12963=ADVANCED_FACE('',(#2251),#12280,.F.);
#12964=ADVANCED_FACE('',(#2252),#12281,.T.);
#12965=ADVANCED_FACE('',(#2253,#1222),#1541,.T.);
#12966=ADVANCED_FACE('',(#2254,#1223),#1542,.F.);
#12967=ADVANCED_FACE('',(#2255),#1543,.F.);
#12968=ADVANCED_FACE('',(#2256),#1544,.T.);
#12969=ADVANCED_FACE('',(#2257),#1545,.T.);
#12970=ADVANCED_FACE('',(#2258),#1546,.T.);
#12971=ADVANCED_FACE('',(#2259),#1547,.T.);
#12972=ADVANCED_FACE('',(#2260),#1548,.T.);
#12973=ADVANCED_FACE('',(#2261),#1549,.F.);
#12974=ADVANCED_FACE('',(#2262),#1550,.T.);
#12975=ADVANCED_FACE('',(#2263),#1551,.T.);
#12976=ADVANCED_FACE('',(#2264),#1552,.T.);
#12977=ADVANCED_FACE('',(#2265),#1553,.F.);
#12978=ADVANCED_FACE('',(#2266),#1554,.F.);
#12979=ADVANCED_FACE('',(#2267),#1555,.F.);
#12980=ADVANCED_FACE('',(#2268),#1556,.F.);
#12981=ADVANCED_FACE('',(#2269),#1557,.F.);
#12982=ADVANCED_FACE('',(#2270),#1558,.F.);
#12983=ADVANCED_FACE('',(#2271),#1559,.F.);
#12984=ADVANCED_FACE('',(#2272,#1224),#1560,.T.);
#12985=ADVANCED_FACE('',(#2273),#801,.T.);
#12986=ADVANCED_FACE('',(#2274),#12282,.T.);
#12987=ADVANCED_FACE('',(#2275),#802,.T.);
#12988=ADVANCED_FACE('',(#2276),#1561,.T.);
#12989=ADVANCED_FACE('',(#2277),#12283,.F.);
#12990=ADVANCED_FACE('',(#2278),#12284,.T.);
#12991=ADVANCED_FACE('',(#2279,#1225),#1562,.T.);
#12992=ADVANCED_FACE('',(#2280,#1226),#1563,.F.);
#12993=ADVANCED_FACE('',(#2281),#1564,.T.);
#12994=ADVANCED_FACE('',(#2282),#803,.T.);
#12995=ADVANCED_FACE('',(#2283),#12285,.T.);
#12996=ADVANCED_FACE('',(#2284),#804,.T.);
#12997=ADVANCED_FACE('',(#2285,#1227),#1565,.T.);
#12998=ADVANCED_FACE('',(#2286),#805,.T.);
#12999=ADVANCED_FACE('',(#2287),#12286,.T.);
#13000=ADVANCED_FACE('',(#2288),#806,.T.);
#13001=ADVANCED_FACE('',(#2289),#1566,.T.);
#13002=ADVANCED_FACE('',(#2290),#1567,.F.);
#13003=ADVANCED_FACE('',(#2291),#1568,.F.);
#13004=ADVANCED_FACE('',(#2292),#1569,.F.);
#13005=ADVANCED_FACE('',(#2293),#1570,.F.);
#13006=ADVANCED_FACE('',(#2294),#1571,.F.);
#13007=ADVANCED_FACE('',(#2295),#1572,.F.);
#13008=ADVANCED_FACE('',(#2296),#1573,.F.);
#13009=ADVANCED_FACE('',(#2297),#1574,.F.);
#13010=CLOSED_SHELL('',(#12287,#12288,#12289,#12290,#12291,#12292,#12293,
#12294,#12295,#12296,#12297,#12298,#12299,#12300,#12301,#12302,#12303,#12304,
#12305,#12306,#12307,#12308));
#13011=CLOSED_SHELL('',(#12309,#12310,#12311,#12312,#12313,#12314,#12315,
#12316,#12317,#12318,#12319,#12320,#12321,#12322,#12323,#12324,#12325,#12326,
#12327,#12328,#12329,#12330));
#13012=CLOSED_SHELL('',(#12331,#12332,#12333,#12334,#12335,#12336,#12337,
#12338,#12339,#12340,#12341,#12342,#12343,#12344,#12345,#12346));
#13013=CLOSED_SHELL('',(#12347,#12348,#12349,#12350,#12351,#12352,#12353,
#12354,#12355));
#13014=CLOSED_SHELL('',(#12356,#12357,#12358,#12359,#12360,#12361,#12362,
#12363,#12364,#12365,#12366,#12367,#12368,#12369,#12370,#12371));
#13015=CLOSED_SHELL('',(#12372,#12373,#12374,#12375,#12376,#12377,#12378,
#12379,#12380,#12381));
#13016=CLOSED_SHELL('',(#12382,#12383,#12384,#12385,#12386,#12387,#12388,
#12389,#12390,#12391,#12392,#12393,#12394,#12395,#12396,#12397));
#13017=CLOSED_SHELL('',(#12398,#12399,#12400,#12401,#12402,#12403,#12404,
#12405,#12406,#12407,#12408,#12409,#12410,#12411,#12412,#12413));
#13018=CLOSED_SHELL('',(#12414,#12415,#12416,#12417,#12418,#12419,#12420,
#12421,#12422,#12423,#12424,#12425,#12426,#12427,#12428,#12429,#12430,#12431,
#12432,#12433,#12434,#12435,#12436,#12437,#12438,#12439));
#13019=CLOSED_SHELL('',(#12440,#12441,#12442,#12443,#12444,#12445,#12446,
#12447));
#13020=CLOSED_SHELL('',(#12448,#12449,#12450,#12451,#12452,#12453,#12454,
#12455));
#13021=CLOSED_SHELL('',(#12456));
#13022=CLOSED_SHELL('',(#12457));
#13023=CLOSED_SHELL('',(#12458));
#13024=CLOSED_SHELL('',(#12459));
#13025=CLOSED_SHELL('',(#12460));
#13026=CLOSED_SHELL('',(#12461));
#13027=CLOSED_SHELL('',(#12462));
#13028=CLOSED_SHELL('',(#12463,#12464,#12465,#12466,#12467,#12468,#12469,
#12470,#12471,#12472,#12473,#12474,#12475,#12476,#12477,#12478,#12479));
#13029=CLOSED_SHELL('',(#12480,#12481,#12482,#12483));
#13030=CLOSED_SHELL('',(#12484,#12485,#12486,#12487));
#13031=CLOSED_SHELL('',(#12488,#12489,#12490,#12491,#12492,#12493,#12494,
#12495));
#13032=CLOSED_SHELL('',(#12496,#12497,#12498,#12499,#12500,#12501,#12502,
#12503));
#13033=CLOSED_SHELL('',(#12504));
#13034=CLOSED_SHELL('',(#12505));
#13035=CLOSED_SHELL('',(#12506));
#13036=CLOSED_SHELL('',(#12507));
#13037=CLOSED_SHELL('',(#12508));
#13038=CLOSED_SHELL('',(#12509));
#13039=CLOSED_SHELL('',(#12510));
#13040=CLOSED_SHELL('',(#12511));
#13041=CLOSED_SHELL('',(#12512,#12513,#12514,#12515,#12516,#12517,#12518,
#12519,#12520,#12521,#12522,#12523,#12524,#12525,#12526,#12527,#12528,#12529,
#12530));
#13042=CLOSED_SHELL('',(#12531,#12532,#12533,#12534));
#13043=CLOSED_SHELL('',(#12535,#12536,#12537,#12538));
#13044=CLOSED_SHELL('',(#12539,#12540,#12541,#12542,#12543,#12544,#12545,
#12546,#12547,#12548,#12549,#12550,#12551,#12552,#12553,#12554,#12555,#12556,
#12557,#12558,#12559,#12560,#12561,#12562,#12563,#12564,#12565,#12566,#12567,
#12568,#12569,#12570,#12571,#12572,#12573,#12574,#12575,#12576,#12577,#12578,
#12579,#12580,#12581,#12582,#12583,#12584,#12585));
#13045=CLOSED_SHELL('',(#12586,#12587,#12588,#12589,#12590,#12591,#12592,
#12593,#12594,#12595));
#13046=CLOSED_SHELL('',(#12596,#12597,#12598,#12599,#12600));
#13047=CLOSED_SHELL('',(#12601,#12602,#12603,#12604,#12605,#12606,#12607,
#12608));
#13048=CLOSED_SHELL('',(#12609,#12610,#12611,#12612,#12613,#12614,#12615,
#12616));
#13049=CLOSED_SHELL('',(#12617,#12618,#12619,#12620,#12621,#12622,#12623,
#12624,#12625,#12626));
#13050=CLOSED_SHELL('',(#12627,#12628,#12629,#12630,#12631,#12632,#12633,
#12634,#12635,#12636,#12637,#12638,#12639,#12640));
#13051=CLOSED_SHELL('',(#12641,#12642,#12643,#12644,#12645,#12646,#12647,
#12648,#12649,#12650,#12651,#12652,#12653,#12654,#12655,#12656,#12657,#12658,
#12659,#12660,#12661));
#13052=CLOSED_SHELL('',(#12662,#12663,#12664,#12665,#12666,#12667,#12668,
#12669,#12670,#12671,#12672,#12673,#12674,#12675,#12676,#12677,#12678,#12679,
#12680,#12681,#12682,#12683));
#13053=CLOSED_SHELL('',(#12684,#12685,#12686,#12687,#12688,#12689,#12690,
#12691,#12692,#12693));
#13054=CLOSED_SHELL('',(#12694,#12695,#12696,#12697,#12698,#12699,#12700,
#12701,#12702,#12703));
#13055=CLOSED_SHELL('',(#12704,#12705,#12706,#12707,#12708));
#13056=CLOSED_SHELL('',(#12709,#12710,#12711,#12712,#12713,#12714,#12715,
#12716));
#13057=CLOSED_SHELL('',(#12717,#12718,#12719,#12720,#12721,#12722,#12723,
#12724,#12725,#12726));
#13058=CLOSED_SHELL('',(#12727,#12728,#12729,#12730,#12731,#12732,#12733,
#12734,#12735,#12736,#12737,#12738,#12739,#12740,#12741,#12742,#12743,#12744,
#12745,#12746,#12747,#12748,#12749,#12750,#12751,#12752,#12753,#12754,#12755,
#12756,#12757));
#13059=CLOSED_SHELL('',(#12758,#12759,#12760,#12761,#12762,#12763,#12764,
#12765,#12766));
#13060=CLOSED_SHELL('',(#12767,#12768,#12769,#12770,#12771,#12772,#12773,
#12774));
#13061=CLOSED_SHELL('',(#12775,#12776,#12777,#12778,#12779,#12780,#12781,
#12782,#12783));
#13062=CLOSED_SHELL('',(#12784,#12785,#12786,#12787,#12788,#12789,#12790,
#12791));
#13063=CLOSED_SHELL('',(#12792,#12793,#12794,#12795,#12796,#12797,#12798,
#12799,#12800,#12801,#12802,#12803,#12804,#12805,#12806,#12807,#12808,#12809,
#12810,#12811,#12812,#12813,#12814,#12815,#12816,#12817,#12818,#12819,#12820,
#12821,#12822,#12823,#12824,#12825,#12826,#12827,#12828,#12829,#12830,#12831,
#12832,#12833,#12834,#12835,#12836,#12837,#12838,#12839,#12840,#12841,#12842,
#12843,#12844,#12845,#12846,#12847,#12848,#12849,#12850,#12851,#12852,#12853,
#12854,#12855,#12856,#12857,#12858,#12859,#12860,#12861,#12862,#12863,#12864,
#12865,#12866,#12867,#12868,#12869,#12870,#12871,#12872,#12873,#12874,#12875,
#12876,#12877,#12878,#12879,#12880,#12881,#12882,#12883,#12884,#12885,#12886,
#12887,#12888,#12889,#12890,#12891,#12892,#12893,#12894,#12895,#12896,#12897,
#12898,#12899,#12900,#12901,#12902,#12903,#12904,#12905,#12906,#12907,#12908,
#12909,#12910,#12911,#12912,#12913,#12914,#12915,#12916,#12917,#12918,#12919,
#12920,#12921,#12922,#12923,#12924,#12925,#12926,#12927,#12928,#12929,#12930,
#12931,#12932,#12933,#12934));
#13064=CLOSED_SHELL('',(#12935,#12936,#12937,#12938));
#13065=CLOSED_SHELL('',(#12939,#12940,#12941,#12942,#12943,#12944,#12945));
#13066=CLOSED_SHELL('',(#12946,#12947,#12948,#12949,#12950,#12951,#12952,
#12953,#12954,#12955,#12956,#12957,#12958));
#13067=CLOSED_SHELL('',(#12959,#12960,#12961,#12962));
#13068=CLOSED_SHELL('',(#12963,#12964,#12965,#12966));
#13069=CLOSED_SHELL('',(#12967,#12968,#12969,#12970,#12971,#12972,#12973,
#12974,#12975,#12976));
#13070=CLOSED_SHELL('',(#12977,#12978,#12979,#12980,#12981,#12982,#12983,
#12984,#12985,#12986,#12987,#12988));
#13071=CLOSED_SHELL('',(#12989,#12990,#12991,#12992));
#13072=CLOSED_SHELL('',(#12993,#12994,#12995,#12996,#12997,#12998,#12999,
#13000,#13001));
#13073=CLOSED_SHELL('',(#13002,#13003,#13004,#13005,#13006,#13007,#13008,
#13009));
#13074=DERIVED_UNIT_ELEMENT(#13162,1.);
#13075=DERIVED_UNIT_ELEMENT(#33983,-3.);
#13076=DERIVED_UNIT_ELEMENT(#13162,1.);
#13077=DERIVED_UNIT_ELEMENT(#33983,-3.);
#13078=DERIVED_UNIT_ELEMENT(#13162,1.);
#13079=DERIVED_UNIT_ELEMENT(#33983,-3.);
#13080=DERIVED_UNIT_ELEMENT(#13162,1.);
#13081=DERIVED_UNIT_ELEMENT(#33983,-3.);
#13082=DERIVED_UNIT_ELEMENT(#13162,1.);
#13083=DERIVED_UNIT_ELEMENT(#33983,-3.);
#13084=DERIVED_UNIT_ELEMENT(#13162,1.);
#13085=DERIVED_UNIT_ELEMENT(#33983,-3.);
#13086=DERIVED_UNIT_ELEMENT(#13162,1.);
#13087=DERIVED_UNIT_ELEMENT(#33983,-3.);
#13088=DERIVED_UNIT_ELEMENT(#13162,1.);
#13089=DERIVED_UNIT_ELEMENT(#33983,-3.);
#13090=DERIVED_UNIT_ELEMENT(#13162,1.);
#13091=DERIVED_UNIT_ELEMENT(#33983,-3.);
#13092=DERIVED_UNIT_ELEMENT(#13162,1.);
#13093=DERIVED_UNIT_ELEMENT(#33983,-3.);
#13094=DERIVED_UNIT_ELEMENT(#13162,1.);
#13095=DERIVED_UNIT_ELEMENT(#33983,-3.);
#13096=DERIVED_UNIT_ELEMENT(#13162,1.);
#13097=DERIVED_UNIT_ELEMENT(#33983,-3.);
#13098=DERIVED_UNIT_ELEMENT(#13162,1.);
#13099=DERIVED_UNIT_ELEMENT(#33983,-3.);
#13100=DERIVED_UNIT_ELEMENT(#13162,1.);
#13101=DERIVED_UNIT_ELEMENT(#33983,-3.);
#13102=DERIVED_UNIT_ELEMENT(#13162,1.);
#13103=DERIVED_UNIT_ELEMENT(#33983,-3.);
#13104=DERIVED_UNIT_ELEMENT(#13162,1.);
#13105=DERIVED_UNIT_ELEMENT(#33983,-3.);
#13106=DERIVED_UNIT_ELEMENT(#13162,1.);
#13107=DERIVED_UNIT_ELEMENT(#33983,-3.);
#13108=DERIVED_UNIT_ELEMENT(#13162,1.);
#13109=DERIVED_UNIT_ELEMENT(#33983,-3.);
#13110=DERIVED_UNIT_ELEMENT(#13162,1.);
#13111=DERIVED_UNIT_ELEMENT(#33983,-3.);
#13112=DERIVED_UNIT_ELEMENT(#13162,1.);
#13113=DERIVED_UNIT_ELEMENT(#33983,-3.);
#13114=DERIVED_UNIT_ELEMENT(#13162,1.);
#13115=DERIVED_UNIT_ELEMENT(#33983,-3.);
#13116=DERIVED_UNIT_ELEMENT(#13162,1.);
#13117=DERIVED_UNIT_ELEMENT(#33983,-3.);
#13118=DERIVED_UNIT_ELEMENT(#13162,1.);
#13119=DERIVED_UNIT_ELEMENT(#33983,-3.);
#13120=DERIVED_UNIT_ELEMENT(#13162,1.);
#13121=DERIVED_UNIT_ELEMENT(#33983,-3.);
#13122=DERIVED_UNIT_ELEMENT(#13162,1.);
#13123=DERIVED_UNIT_ELEMENT(#33983,-3.);
#13124=DERIVED_UNIT_ELEMENT(#13162,1.);
#13125=DERIVED_UNIT_ELEMENT(#33983,-3.);
#13126=DERIVED_UNIT_ELEMENT(#13162,1.);
#13127=DERIVED_UNIT_ELEMENT(#33983,-3.);
#13128=DERIVED_UNIT_ELEMENT(#13162,1.);
#13129=DERIVED_UNIT_ELEMENT(#33983,-3.);
#13130=DERIVED_UNIT_ELEMENT(#13162,1.);
#13131=DERIVED_UNIT_ELEMENT(#33983,-3.);
#13132=DERIVED_UNIT_ELEMENT(#13162,1.);
#13133=DERIVED_UNIT_ELEMENT(#33983,-3.);
#13134=DERIVED_UNIT_ELEMENT(#13162,1.);
#13135=DERIVED_UNIT_ELEMENT(#33983,-3.);
#13136=DERIVED_UNIT_ELEMENT(#13162,1.);
#13137=DERIVED_UNIT_ELEMENT(#33983,-3.);
#13138=DERIVED_UNIT_ELEMENT(#13162,1.);
#13139=DERIVED_UNIT_ELEMENT(#33983,-3.);
#13140=DERIVED_UNIT_ELEMENT(#13162,1.);
#13141=DERIVED_UNIT_ELEMENT(#33983,-3.);
#13142=DERIVED_UNIT_ELEMENT(#13162,1.);
#13143=DERIVED_UNIT_ELEMENT(#33983,-3.);
#13144=DERIVED_UNIT_ELEMENT(#13162,1.);
#13145=DERIVED_UNIT_ELEMENT(#33983,-3.);
#13146=DERIVED_UNIT_ELEMENT(#13162,1.);
#13147=DERIVED_UNIT_ELEMENT(#33983,-3.);
#13148=DERIVED_UNIT_ELEMENT(#13162,1.);
#13149=DERIVED_UNIT_ELEMENT(#33983,-3.);
#13150=DERIVED_UNIT_ELEMENT(#13162,1.);
#13151=DERIVED_UNIT_ELEMENT(#33983,-3.);
#13152=DERIVED_UNIT_ELEMENT(#13162,1.);
#13153=DERIVED_UNIT_ELEMENT(#33983,-3.);
#13154=DERIVED_UNIT_ELEMENT(#13162,1.);
#13155=DERIVED_UNIT_ELEMENT(#33983,-3.);
#13156=DERIVED_UNIT_ELEMENT(#13162,1.);
#13157=DERIVED_UNIT_ELEMENT(#33983,-3.);
#13158=DERIVED_UNIT_ELEMENT(#13162,1.);
#13159=DERIVED_UNIT_ELEMENT(#33983,-3.);
#13160=DERIVED_UNIT_ELEMENT(#13162,1.);
#13161=DERIVED_UNIT_ELEMENT(#33983,-3.);
#13162=(
MASS_UNIT()
NAMED_UNIT(*)
SI_UNIT(.KILO.,.GRAM.)
);
#13163=DERIVED_UNIT((#13074,#13075));
#13164=DERIVED_UNIT((#13076,#13077));
#13165=DERIVED_UNIT((#13078,#13079));
#13166=DERIVED_UNIT((#13080,#13081));
#13167=DERIVED_UNIT((#13082,#13083));
#13168=DERIVED_UNIT((#13084,#13085));
#13169=DERIVED_UNIT((#13086,#13087));
#13170=DERIVED_UNIT((#13088,#13089));
#13171=DERIVED_UNIT((#13090,#13091));
#13172=DERIVED_UNIT((#13092,#13093));
#13173=DERIVED_UNIT((#13094,#13095));
#13174=DERIVED_UNIT((#13096,#13097));
#13175=DERIVED_UNIT((#13098,#13099));
#13176=DERIVED_UNIT((#13100,#13101));
#13177=DERIVED_UNIT((#13102,#13103));
#13178=DERIVED_UNIT((#13104,#13105));
#13179=DERIVED_UNIT((#13106,#13107));
#13180=DERIVED_UNIT((#13108,#13109));
#13181=DERIVED_UNIT((#13110,#13111));
#13182=DERIVED_UNIT((#13112,#13113));
#13183=DERIVED_UNIT((#13114,#13115));
#13184=DERIVED_UNIT((#13116,#13117));
#13185=DERIVED_UNIT((#13118,#13119));
#13186=DERIVED_UNIT((#13120,#13121));
#13187=DERIVED_UNIT((#13122,#13123));
#13188=DERIVED_UNIT((#13124,#13125));
#13189=DERIVED_UNIT((#13126,#13127));
#13190=DERIVED_UNIT((#13128,#13129));
#13191=DERIVED_UNIT((#13130,#13131));
#13192=DERIVED_UNIT((#13132,#13133));
#13193=DERIVED_UNIT((#13134,#13135));
#13194=DERIVED_UNIT((#13136,#13137));
#13195=DERIVED_UNIT((#13138,#13139));
#13196=DERIVED_UNIT((#13140,#13141));
#13197=DERIVED_UNIT((#13142,#13143));
#13198=DERIVED_UNIT((#13144,#13145));
#13199=DERIVED_UNIT((#13146,#13147));
#13200=DERIVED_UNIT((#13148,#13149));
#13201=DERIVED_UNIT((#13150,#13151));
#13202=DERIVED_UNIT((#13152,#13153));
#13203=DERIVED_UNIT((#13154,#13155));
#13204=DERIVED_UNIT((#13156,#13157));
#13205=DERIVED_UNIT((#13158,#13159));
#13206=DERIVED_UNIT((#13160,#13161));
#13207=MEASURE_REPRESENTATION_ITEM('density measure',
POSITIVE_RATIO_MEASURE(7850.),#13163);
#13208=MEASURE_REPRESENTATION_ITEM('density measure',
POSITIVE_RATIO_MEASURE(7850.),#13164);
#13209=MEASURE_REPRESENTATION_ITEM('density measure',
POSITIVE_RATIO_MEASURE(7850.),#13165);
#13210=MEASURE_REPRESENTATION_ITEM('density measure',
POSITIVE_RATIO_MEASURE(7850.),#13166);
#13211=MEASURE_REPRESENTATION_ITEM('density measure',
POSITIVE_RATIO_MEASURE(7850.),#13167);
#13212=MEASURE_REPRESENTATION_ITEM('density measure',
POSITIVE_RATIO_MEASURE(7850.),#13168);
#13213=MEASURE_REPRESENTATION_ITEM('density measure',
POSITIVE_RATIO_MEASURE(7850.),#13169);
#13214=MEASURE_REPRESENTATION_ITEM('density measure',
POSITIVE_RATIO_MEASURE(7850.),#13170);
#13215=MEASURE_REPRESENTATION_ITEM('density measure',
POSITIVE_RATIO_MEASURE(7850.),#13171);
#13216=MEASURE_REPRESENTATION_ITEM('density measure',
POSITIVE_RATIO_MEASURE(7850.),#13172);
#13217=MEASURE_REPRESENTATION_ITEM('density measure',
POSITIVE_RATIO_MEASURE(7850.),#13173);
#13218=MEASURE_REPRESENTATION_ITEM('density measure',
POSITIVE_RATIO_MEASURE(7850.),#13174);
#13219=MEASURE_REPRESENTATION_ITEM('density measure',
POSITIVE_RATIO_MEASURE(7850.),#13175);
#13220=MEASURE_REPRESENTATION_ITEM('density measure',
POSITIVE_RATIO_MEASURE(7850.),#13176);
#13221=MEASURE_REPRESENTATION_ITEM('density measure',
POSITIVE_RATIO_MEASURE(7850.),#13177);
#13222=MEASURE_REPRESENTATION_ITEM('density measure',
POSITIVE_RATIO_MEASURE(7850.),#13178);
#13223=MEASURE_REPRESENTATION_ITEM('density measure',
POSITIVE_RATIO_MEASURE(7850.),#13179);
#13224=MEASURE_REPRESENTATION_ITEM('density measure',
POSITIVE_RATIO_MEASURE(7850.),#13180);
#13225=MEASURE_REPRESENTATION_ITEM('density measure',
POSITIVE_RATIO_MEASURE(7850.),#13181);
#13226=MEASURE_REPRESENTATION_ITEM('density measure',
POSITIVE_RATIO_MEASURE(7850.),#13182);
#13227=MEASURE_REPRESENTATION_ITEM('density measure',
POSITIVE_RATIO_MEASURE(7850.),#13183);
#13228=MEASURE_REPRESENTATION_ITEM('density measure',
POSITIVE_RATIO_MEASURE(7850.),#13184);
#13229=MEASURE_REPRESENTATION_ITEM('density measure',
POSITIVE_RATIO_MEASURE(7850.),#13185);
#13230=MEASURE_REPRESENTATION_ITEM('density measure',
POSITIVE_RATIO_MEASURE(7850.),#13186);
#13231=MEASURE_REPRESENTATION_ITEM('density measure',
POSITIVE_RATIO_MEASURE(7850.),#13187);
#13232=MEASURE_REPRESENTATION_ITEM('density measure',
POSITIVE_RATIO_MEASURE(7850.),#13188);
#13233=MEASURE_REPRESENTATION_ITEM('density measure',
POSITIVE_RATIO_MEASURE(7850.),#13189);
#13234=MEASURE_REPRESENTATION_ITEM('density measure',
POSITIVE_RATIO_MEASURE(7850.),#13190);
#13235=MEASURE_REPRESENTATION_ITEM('density measure',
POSITIVE_RATIO_MEASURE(7850.),#13191);
#13236=MEASURE_REPRESENTATION_ITEM('density measure',
POSITIVE_RATIO_MEASURE(7850.),#13192);
#13237=MEASURE_REPRESENTATION_ITEM('density measure',
POSITIVE_RATIO_MEASURE(7850.),#13193);
#13238=MEASURE_REPRESENTATION_ITEM('density measure',
POSITIVE_RATIO_MEASURE(7850.),#13194);
#13239=MEASURE_REPRESENTATION_ITEM('density measure',
POSITIVE_RATIO_MEASURE(7850.),#13195);
#13240=MEASURE_REPRESENTATION_ITEM('density measure',
POSITIVE_RATIO_MEASURE(7850.),#13196);
#13241=MEASURE_REPRESENTATION_ITEM('density measure',
POSITIVE_RATIO_MEASURE(7850.),#13197);
#13242=MEASURE_REPRESENTATION_ITEM('density measure',
POSITIVE_RATIO_MEASURE(7850.),#13198);
#13243=MEASURE_REPRESENTATION_ITEM('density measure',
POSITIVE_RATIO_MEASURE(7850.),#13199);
#13244=MEASURE_REPRESENTATION_ITEM('density measure',
POSITIVE_RATIO_MEASURE(7850.),#13200);
#13245=MEASURE_REPRESENTATION_ITEM('density measure',
POSITIVE_RATIO_MEASURE(7850.),#13201);
#13246=MEASURE_REPRESENTATION_ITEM('density measure',
POSITIVE_RATIO_MEASURE(7850.),#13202);
#13247=MEASURE_REPRESENTATION_ITEM('density measure',
POSITIVE_RATIO_MEASURE(7850.),#13203);
#13248=MEASURE_REPRESENTATION_ITEM('density measure',
POSITIVE_RATIO_MEASURE(7850.),#13204);
#13249=MEASURE_REPRESENTATION_ITEM('density measure',
POSITIVE_RATIO_MEASURE(7850.),#13205);
#13250=MEASURE_REPRESENTATION_ITEM('density measure',
POSITIVE_RATIO_MEASURE(7850.),#13206);
#13251=PROPERTY_DEFINITION_REPRESENTATION(#13471,#13339);
#13252=PROPERTY_DEFINITION_REPRESENTATION(#13472,#13340);
#13253=PROPERTY_DEFINITION_REPRESENTATION(#13473,#13341);
#13254=PROPERTY_DEFINITION_REPRESENTATION(#13474,#13342);
#13255=PROPERTY_DEFINITION_REPRESENTATION(#13475,#13343);
#13256=PROPERTY_DEFINITION_REPRESENTATION(#13476,#13344);
#13257=PROPERTY_DEFINITION_REPRESENTATION(#13477,#13345);
#13258=PROPERTY_DEFINITION_REPRESENTATION(#13478,#13346);
#13259=PROPERTY_DEFINITION_REPRESENTATION(#13479,#13347);
#13260=PROPERTY_DEFINITION_REPRESENTATION(#13480,#13348);
#13261=PROPERTY_DEFINITION_REPRESENTATION(#13481,#13349);
#13262=PROPERTY_DEFINITION_REPRESENTATION(#13482,#13350);
#13263=PROPERTY_DEFINITION_REPRESENTATION(#13483,#13351);
#13264=PROPERTY_DEFINITION_REPRESENTATION(#13484,#13352);
#13265=PROPERTY_DEFINITION_REPRESENTATION(#13485,#13353);
#13266=PROPERTY_DEFINITION_REPRESENTATION(#13486,#13354);
#13267=PROPERTY_DEFINITION_REPRESENTATION(#13487,#13355);
#13268=PROPERTY_DEFINITION_REPRESENTATION(#13488,#13356);
#13269=PROPERTY_DEFINITION_REPRESENTATION(#13489,#13357);
#13270=PROPERTY_DEFINITION_REPRESENTATION(#13490,#13358);
#13271=PROPERTY_DEFINITION_REPRESENTATION(#13491,#13359);
#13272=PROPERTY_DEFINITION_REPRESENTATION(#13492,#13360);
#13273=PROPERTY_DEFINITION_REPRESENTATION(#13493,#13361);
#13274=PROPERTY_DEFINITION_REPRESENTATION(#13494,#13362);
#13275=PROPERTY_DEFINITION_REPRESENTATION(#13495,#13363);
#13276=PROPERTY_DEFINITION_REPRESENTATION(#13496,#13364);
#13277=PROPERTY_DEFINITION_REPRESENTATION(#13497,#13365);
#13278=PROPERTY_DEFINITION_REPRESENTATION(#13498,#13366);
#13279=PROPERTY_DEFINITION_REPRESENTATION(#13499,#13367);
#13280=PROPERTY_DEFINITION_REPRESENTATION(#13500,#13368);
#13281=PROPERTY_DEFINITION_REPRESENTATION(#13501,#13369);
#13282=PROPERTY_DEFINITION_REPRESENTATION(#13502,#13370);
#13283=PROPERTY_DEFINITION_REPRESENTATION(#13503,#13371);
#13284=PROPERTY_DEFINITION_REPRESENTATION(#13504,#13372);
#13285=PROPERTY_DEFINITION_REPRESENTATION(#13505,#13373);
#13286=PROPERTY_DEFINITION_REPRESENTATION(#13506,#13374);
#13287=PROPERTY_DEFINITION_REPRESENTATION(#13507,#13375);
#13288=PROPERTY_DEFINITION_REPRESENTATION(#13508,#13376);
#13289=PROPERTY_DEFINITION_REPRESENTATION(#13509,#13377);
#13290=PROPERTY_DEFINITION_REPRESENTATION(#13510,#13378);
#13291=PROPERTY_DEFINITION_REPRESENTATION(#13511,#13379);
#13292=PROPERTY_DEFINITION_REPRESENTATION(#13512,#13380);
#13293=PROPERTY_DEFINITION_REPRESENTATION(#13513,#13381);
#13294=PROPERTY_DEFINITION_REPRESENTATION(#13514,#13382);
#13295=PROPERTY_DEFINITION_REPRESENTATION(#13515,#13383);
#13296=PROPERTY_DEFINITION_REPRESENTATION(#13516,#13384);
#13297=PROPERTY_DEFINITION_REPRESENTATION(#13517,#13385);
#13298=PROPERTY_DEFINITION_REPRESENTATION(#13518,#13386);
#13299=PROPERTY_DEFINITION_REPRESENTATION(#13519,#13387);
#13300=PROPERTY_DEFINITION_REPRESENTATION(#13520,#13388);
#13301=PROPERTY_DEFINITION_REPRESENTATION(#13521,#13389);
#13302=PROPERTY_DEFINITION_REPRESENTATION(#13522,#13390);
#13303=PROPERTY_DEFINITION_REPRESENTATION(#13523,#13391);
#13304=PROPERTY_DEFINITION_REPRESENTATION(#13524,#13392);
#13305=PROPERTY_DEFINITION_REPRESENTATION(#13525,#13393);
#13306=PROPERTY_DEFINITION_REPRESENTATION(#13526,#13394);
#13307=PROPERTY_DEFINITION_REPRESENTATION(#13527,#13395);
#13308=PROPERTY_DEFINITION_REPRESENTATION(#13528,#13396);
#13309=PROPERTY_DEFINITION_REPRESENTATION(#13529,#13397);
#13310=PROPERTY_DEFINITION_REPRESENTATION(#13530,#13398);
#13311=PROPERTY_DEFINITION_REPRESENTATION(#13531,#13399);
#13312=PROPERTY_DEFINITION_REPRESENTATION(#13532,#13400);
#13313=PROPERTY_DEFINITION_REPRESENTATION(#13533,#13401);
#13314=PROPERTY_DEFINITION_REPRESENTATION(#13534,#13402);
#13315=PROPERTY_DEFINITION_REPRESENTATION(#13535,#13403);
#13316=PROPERTY_DEFINITION_REPRESENTATION(#13536,#13404);
#13317=PROPERTY_DEFINITION_REPRESENTATION(#13537,#13405);
#13318=PROPERTY_DEFINITION_REPRESENTATION(#13538,#13406);
#13319=PROPERTY_DEFINITION_REPRESENTATION(#13539,#13407);
#13320=PROPERTY_DEFINITION_REPRESENTATION(#13540,#13408);
#13321=PROPERTY_DEFINITION_REPRESENTATION(#13541,#13409);
#13322=PROPERTY_DEFINITION_REPRESENTATION(#13542,#13410);
#13323=PROPERTY_DEFINITION_REPRESENTATION(#13543,#13411);
#13324=PROPERTY_DEFINITION_REPRESENTATION(#13544,#13412);
#13325=PROPERTY_DEFINITION_REPRESENTATION(#13545,#13413);
#13326=PROPERTY_DEFINITION_REPRESENTATION(#13546,#13414);
#13327=PROPERTY_DEFINITION_REPRESENTATION(#13547,#13415);
#13328=PROPERTY_DEFINITION_REPRESENTATION(#13548,#13416);
#13329=PROPERTY_DEFINITION_REPRESENTATION(#13549,#13417);
#13330=PROPERTY_DEFINITION_REPRESENTATION(#13550,#13418);
#13331=PROPERTY_DEFINITION_REPRESENTATION(#13551,#13419);
#13332=PROPERTY_DEFINITION_REPRESENTATION(#13552,#13420);
#13333=PROPERTY_DEFINITION_REPRESENTATION(#13553,#13421);
#13334=PROPERTY_DEFINITION_REPRESENTATION(#13554,#13422);
#13335=PROPERTY_DEFINITION_REPRESENTATION(#13555,#13423);
#13336=PROPERTY_DEFINITION_REPRESENTATION(#13556,#13424);
#13337=PROPERTY_DEFINITION_REPRESENTATION(#13557,#13425);
#13338=PROPERTY_DEFINITION_REPRESENTATION(#13558,#13426);
#13339=REPRESENTATION('material name',(#13427),#33932);
#13340=REPRESENTATION('density',(#13207),#33932);
#13341=REPRESENTATION('material name',(#13428),#33933);
#13342=REPRESENTATION('density',(#13208),#33933);
#13343=REPRESENTATION('material name',(#13429),#33934);
#13344=REPRESENTATION('density',(#13209),#33934);
#13345=REPRESENTATION('material name',(#13430),#33935);
#13346=REPRESENTATION('density',(#13210),#33935);
#13347=REPRESENTATION('material name',(#13431),#33936);
#13348=REPRESENTATION('density',(#13211),#33936);
#13349=REPRESENTATION('material name',(#13432),#33937);
#13350=REPRESENTATION('density',(#13212),#33937);
#13351=REPRESENTATION('material name',(#13433),#33938);
#13352=REPRESENTATION('density',(#13213),#33938);
#13353=REPRESENTATION('material name',(#13434),#33939);
#13354=REPRESENTATION('density',(#13214),#33939);
#13355=REPRESENTATION('material name',(#13435),#33940);
#13356=REPRESENTATION('density',(#13215),#33940);
#13357=REPRESENTATION('material name',(#13436),#33942);
#13358=REPRESENTATION('density',(#13216),#33942);
#13359=REPRESENTATION('material name',(#13437),#33943);
#13360=REPRESENTATION('density',(#13217),#33943);
#13361=REPRESENTATION('material name',(#13438),#33944);
#13362=REPRESENTATION('density',(#13218),#33944);
#13363=REPRESENTATION('material name',(#13439),#33945);
#13364=REPRESENTATION('density',(#13219),#33945);
#13365=REPRESENTATION('material name',(#13440),#33946);
#13366=REPRESENTATION('density',(#13220),#33946);
#13367=REPRESENTATION('material name',(#13441),#33948);
#13368=REPRESENTATION('density',(#13221),#33948);
#13369=REPRESENTATION('material name',(#13442),#33949);
#13370=REPRESENTATION('density',(#13222),#33949);
#13371=REPRESENTATION('material name',(#13443),#33950);
#13372=REPRESENTATION('density',(#13223),#33950);
#13373=REPRESENTATION('material name',(#13444),#33951);
#13374=REPRESENTATION('density',(#13224),#33951);
#13375=REPRESENTATION('material name',(#13445),#33952);
#13376=REPRESENTATION('density',(#13225),#33952);
#13377=REPRESENTATION('material name',(#13446),#33953);
#13378=REPRESENTATION('density',(#13226),#33953);
#13379=REPRESENTATION('material name',(#13447),#33954);
#13380=REPRESENTATION('density',(#13227),#33954);
#13381=REPRESENTATION('material name',(#13448),#33955);
#13382=REPRESENTATION('density',(#13228),#33955);
#13383=REPRESENTATION('material name',(#13449),#33956);
#13384=REPRESENTATION('density',(#13229),#33956);
#13385=REPRESENTATION('material name',(#13450),#33958);
#13386=REPRESENTATION('density',(#13230),#33958);
#13387=REPRESENTATION('material name',(#13451),#33959);
#13388=REPRESENTATION('density',(#13231),#33959);
#13389=REPRESENTATION('material name',(#13452),#33960);
#13390=REPRESENTATION('density',(#13232),#33960);
#13391=REPRESENTATION('material name',(#13453),#33962);
#13392=REPRESENTATION('density',(#13233),#33962);
#13393=REPRESENTATION('material name',(#13454),#33963);
#13394=REPRESENTATION('density',(#13234),#33963);
#13395=REPRESENTATION('material name',(#13455),#33964);
#13396=REPRESENTATION('density',(#13235),#33964);
#13397=REPRESENTATION('material name',(#13456),#33965);
#13398=REPRESENTATION('density',(#13236),#33965);
#13399=REPRESENTATION('material name',(#13457),#33966);
#13400=REPRESENTATION('density',(#13237),#33966);
#13401=REPRESENTATION('material name',(#13458),#33967);
#13402=REPRESENTATION('density',(#13238),#33967);
#13403=REPRESENTATION('material name',(#13459),#33968);
#13404=REPRESENTATION('density',(#13239),#33968);
#13405=REPRESENTATION('material name',(#13460),#33969);
#13406=REPRESENTATION('density',(#13240),#33969);
#13407=REPRESENTATION('material name',(#13461),#33971);
#13408=REPRESENTATION('density',(#13241),#33971);
#13409=REPRESENTATION('material name',(#13462),#33972);
#13410=REPRESENTATION('density',(#13242),#33972);
#13411=REPRESENTATION('material name',(#13463),#33973);
#13412=REPRESENTATION('density',(#13243),#33973);
#13413=REPRESENTATION('material name',(#13464),#33974);
#13414=REPRESENTATION('density',(#13244),#33974);
#13415=REPRESENTATION('material name',(#13465),#33975);
#13416=REPRESENTATION('density',(#13245),#33975);
#13417=REPRESENTATION('material name',(#13466),#33976);
#13418=REPRESENTATION('density',(#13246),#33976);
#13419=REPRESENTATION('material name',(#13467),#33977);
#13420=REPRESENTATION('density',(#13247),#33977);
#13421=REPRESENTATION('material name',(#13468),#33978);
#13422=REPRESENTATION('density',(#13248),#33978);
#13423=REPRESENTATION('material name',(#13469),#33979);
#13424=REPRESENTATION('density',(#13249),#33979);
#13425=REPRESENTATION('material name',(#13470),#33980);
#13426=REPRESENTATION('density',(#13250),#33980);
#13427=DESCRIPTIVE_REPRESENTATION_ITEM('Steel','Steel');
#13428=DESCRIPTIVE_REPRESENTATION_ITEM('Steel','Steel');
#13429=DESCRIPTIVE_REPRESENTATION_ITEM('Steel','Steel');
#13430=DESCRIPTIVE_REPRESENTATION_ITEM('Steel','Steel');
#13431=DESCRIPTIVE_REPRESENTATION_ITEM('Steel','Steel');
#13432=DESCRIPTIVE_REPRESENTATION_ITEM('Steel','Steel');
#13433=DESCRIPTIVE_REPRESENTATION_ITEM('Steel','Steel');
#13434=DESCRIPTIVE_REPRESENTATION_ITEM('Steel','Steel');
#13435=DESCRIPTIVE_REPRESENTATION_ITEM('Steel','Steel');
#13436=DESCRIPTIVE_REPRESENTATION_ITEM('Steel','Steel');
#13437=DESCRIPTIVE_REPRESENTATION_ITEM('Steel','Steel');
#13438=DESCRIPTIVE_REPRESENTATION_ITEM('Steel','Steel');
#13439=DESCRIPTIVE_REPRESENTATION_ITEM('Steel','Steel');
#13440=DESCRIPTIVE_REPRESENTATION_ITEM('Steel','Steel');
#13441=DESCRIPTIVE_REPRESENTATION_ITEM('Steel','Steel');
#13442=DESCRIPTIVE_REPRESENTATION_ITEM('Steel','Steel');
#13443=DESCRIPTIVE_REPRESENTATION_ITEM('Steel','Steel');
#13444=DESCRIPTIVE_REPRESENTATION_ITEM('Steel','Steel');
#13445=DESCRIPTIVE_REPRESENTATION_ITEM('Steel','Steel');
#13446=DESCRIPTIVE_REPRESENTATION_ITEM('Steel','Steel');
#13447=DESCRIPTIVE_REPRESENTATION_ITEM('Steel','Steel');
#13448=DESCRIPTIVE_REPRESENTATION_ITEM('Steel','Steel');
#13449=DESCRIPTIVE_REPRESENTATION_ITEM('Steel','Steel');
#13450=DESCRIPTIVE_REPRESENTATION_ITEM('Steel','Steel');
#13451=DESCRIPTIVE_REPRESENTATION_ITEM('Steel','Steel');
#13452=DESCRIPTIVE_REPRESENTATION_ITEM('Steel','Steel');
#13453=DESCRIPTIVE_REPRESENTATION_ITEM('Steel','Steel');
#13454=DESCRIPTIVE_REPRESENTATION_ITEM('Steel','Steel');
#13455=DESCRIPTIVE_REPRESENTATION_ITEM('Steel','Steel');
#13456=DESCRIPTIVE_REPRESENTATION_ITEM('Steel','Steel');
#13457=DESCRIPTIVE_REPRESENTATION_ITEM('Steel','Steel');
#13458=DESCRIPTIVE_REPRESENTATION_ITEM('Steel','Steel');
#13459=DESCRIPTIVE_REPRESENTATION_ITEM('Steel','Steel');
#13460=DESCRIPTIVE_REPRESENTATION_ITEM('Steel','Steel');
#13461=DESCRIPTIVE_REPRESENTATION_ITEM('Steel','Steel');
#13462=DESCRIPTIVE_REPRESENTATION_ITEM('Steel','Steel');
#13463=DESCRIPTIVE_REPRESENTATION_ITEM('Steel','Steel');
#13464=DESCRIPTIVE_REPRESENTATION_ITEM('Steel','Steel');
#13465=DESCRIPTIVE_REPRESENTATION_ITEM('Steel','Steel');
#13466=DESCRIPTIVE_REPRESENTATION_ITEM('Steel','Steel');
#13467=DESCRIPTIVE_REPRESENTATION_ITEM('Steel','Steel');
#13468=DESCRIPTIVE_REPRESENTATION_ITEM('Steel','Steel');
#13469=DESCRIPTIVE_REPRESENTATION_ITEM('Steel','Steel');
#13470=DESCRIPTIVE_REPRESENTATION_ITEM('Steel','Steel');
#13471=PROPERTY_DEFINITION('material property','material name',#34236);
#13472=PROPERTY_DEFINITION('material property','density of part',#34236);
#13473=PROPERTY_DEFINITION('material property','material name',#34237);
#13474=PROPERTY_DEFINITION('material property','density of part',#34237);
#13475=PROPERTY_DEFINITION('material property','material name',#34238);
#13476=PROPERTY_DEFINITION('material property','density of part',#34238);
#13477=PROPERTY_DEFINITION('material property','material name',#34239);
#13478=PROPERTY_DEFINITION('material property','density of part',#34239);
#13479=PROPERTY_DEFINITION('material property','material name',#34240);
#13480=PROPERTY_DEFINITION('material property','density of part',#34240);
#13481=PROPERTY_DEFINITION('material property','material name',#34241);
#13482=PROPERTY_DEFINITION('material property','density of part',#34241);
#13483=PROPERTY_DEFINITION('material property','material name',#34242);
#13484=PROPERTY_DEFINITION('material property','density of part',#34242);
#13485=PROPERTY_DEFINITION('material property','material name',#34243);
#13486=PROPERTY_DEFINITION('material property','density of part',#34243);
#13487=PROPERTY_DEFINITION('material property','material name',#34244);
#13488=PROPERTY_DEFINITION('material property','density of part',#34244);
#13489=PROPERTY_DEFINITION('material property','material name',#34246);
#13490=PROPERTY_DEFINITION('material property','density of part',#34246);
#13491=PROPERTY_DEFINITION('material property','material name',#34247);
#13492=PROPERTY_DEFINITION('material property','density of part',#34247);
#13493=PROPERTY_DEFINITION('material property','material name',#34248);
#13494=PROPERTY_DEFINITION('material property','density of part',#34248);
#13495=PROPERTY_DEFINITION('material property','material name',#34249);
#13496=PROPERTY_DEFINITION('material property','density of part',#34249);
#13497=PROPERTY_DEFINITION('material property','material name',#34250);
#13498=PROPERTY_DEFINITION('material property','density of part',#34250);
#13499=PROPERTY_DEFINITION('material property','material name',#34252);
#13500=PROPERTY_DEFINITION('material property','density of part',#34252);
#13501=PROPERTY_DEFINITION('material property','material name',#34253);
#13502=PROPERTY_DEFINITION('material property','density of part',#34253);
#13503=PROPERTY_DEFINITION('material property','material name',#34254);
#13504=PROPERTY_DEFINITION('material property','density of part',#34254);
#13505=PROPERTY_DEFINITION('material property','material name',#34255);
#13506=PROPERTY_DEFINITION('material property','density of part',#34255);
#13507=PROPERTY_DEFINITION('material property','material name',#34256);
#13508=PROPERTY_DEFINITION('material property','density of part',#34256);
#13509=PROPERTY_DEFINITION('material property','material name',#34257);
#13510=PROPERTY_DEFINITION('material property','density of part',#34257);
#13511=PROPERTY_DEFINITION('material property','material name',#34258);
#13512=PROPERTY_DEFINITION('material property','density of part',#34258);
#13513=PROPERTY_DEFINITION('material property','material name',#34259);
#13514=PROPERTY_DEFINITION('material property','density of part',#34259);
#13515=PROPERTY_DEFINITION('material property','material name',#34260);
#13516=PROPERTY_DEFINITION('material property','density of part',#34260);
#13517=PROPERTY_DEFINITION('material property','material name',#34262);
#13518=PROPERTY_DEFINITION('material property','density of part',#34262);
#13519=PROPERTY_DEFINITION('material property','material name',#34263);
#13520=PROPERTY_DEFINITION('material property','density of part',#34263);
#13521=PROPERTY_DEFINITION('material property','material name',#34264);
#13522=PROPERTY_DEFINITION('material property','density of part',#34264);
#13523=PROPERTY_DEFINITION('material property','material name',#34266);
#13524=PROPERTY_DEFINITION('material property','density of part',#34266);
#13525=PROPERTY_DEFINITION('material property','material name',#34267);
#13526=PROPERTY_DEFINITION('material property','density of part',#34267);
#13527=PROPERTY_DEFINITION('material property','material name',#34268);
#13528=PROPERTY_DEFINITION('material property','density of part',#34268);
#13529=PROPERTY_DEFINITION('material property','material name',#34269);
#13530=PROPERTY_DEFINITION('material property','density of part',#34269);
#13531=PROPERTY_DEFINITION('material property','material name',#34270);
#13532=PROPERTY_DEFINITION('material property','density of part',#34270);
#13533=PROPERTY_DEFINITION('material property','material name',#34271);
#13534=PROPERTY_DEFINITION('material property','density of part',#34271);
#13535=PROPERTY_DEFINITION('material property','material name',#34272);
#13536=PROPERTY_DEFINITION('material property','density of part',#34272);
#13537=PROPERTY_DEFINITION('material property','material name',#34273);
#13538=PROPERTY_DEFINITION('material property','density of part',#34273);
#13539=PROPERTY_DEFINITION('material property','material name',#34275);
#13540=PROPERTY_DEFINITION('material property','density of part',#34275);
#13541=PROPERTY_DEFINITION('material property','material name',#34276);
#13542=PROPERTY_DEFINITION('material property','density of part',#34276);
#13543=PROPERTY_DEFINITION('material property','material name',#34277);
#13544=PROPERTY_DEFINITION('material property','density of part',#34277);
#13545=PROPERTY_DEFINITION('material property','material name',#34278);
#13546=PROPERTY_DEFINITION('material property','density of part',#34278);
#13547=PROPERTY_DEFINITION('material property','material name',#34279);
#13548=PROPERTY_DEFINITION('material property','density of part',#34279);
#13549=PROPERTY_DEFINITION('material property','material name',#34280);
#13550=PROPERTY_DEFINITION('material property','density of part',#34280);
#13551=PROPERTY_DEFINITION('material property','material name',#34281);
#13552=PROPERTY_DEFINITION('material property','density of part',#34281);
#13553=PROPERTY_DEFINITION('material property','material name',#34282);
#13554=PROPERTY_DEFINITION('material property','density of part',#34282);
#13555=PROPERTY_DEFINITION('material property','material name',#34283);
#13556=PROPERTY_DEFINITION('material property','density of part',#34283);
#13557=PROPERTY_DEFINITION('material property','material name',#34284);
#13558=PROPERTY_DEFINITION('material property','density of part',#34284);
#13559=AXIS2_PLACEMENT_3D('',#18486,#14890,#14891);
#13560=AXIS2_PLACEMENT_3D('',#18487,#14892,#14893);
#13561=AXIS2_PLACEMENT_3D('',#18488,#14894,#14895);
#13562=AXIS2_PLACEMENT_3D('',#18489,#14896,#14897);
#13563=AXIS2_PLACEMENT_3D('',#18491,#14898,#14899);
#13564=AXIS2_PLACEMENT_3D('',#18494,#14901,#14902);
#13565=AXIS2_PLACEMENT_3D('',#18495,#14903,#14904);
#13566=AXIS2_PLACEMENT_3D('',#18497,#14905,#14906);
#13567=AXIS2_PLACEMENT_3D('',#18500,#14908,#14909);
#13568=AXIS2_PLACEMENT_3D('',#18501,#14910,#14911);
#13569=AXIS2_PLACEMENT_3D('',#18503,#14912,#14913);
#13570=AXIS2_PLACEMENT_3D('',#18506,#14915,#14916);
#13571=AXIS2_PLACEMENT_3D('',#18507,#14917,#14918);
#13572=AXIS2_PLACEMENT_3D('',#18509,#14919,#14920);
#13573=AXIS2_PLACEMENT_3D('',#18512,#14922,#14923);
#13574=AXIS2_PLACEMENT_3D('',#18513,#14924,#14925);
#13575=AXIS2_PLACEMENT_3D('',#18515,#14926,#14927);
#13576=AXIS2_PLACEMENT_3D('',#18518,#14929,#14930);
#13577=AXIS2_PLACEMENT_3D('',#18519,#14931,#14932);
#13578=AXIS2_PLACEMENT_3D('',#18521,#14933,#14934);
#13579=AXIS2_PLACEMENT_3D('',#18524,#14936,#14937);
#13580=AXIS2_PLACEMENT_3D('',#18525,#14938,#14939);
#13581=AXIS2_PLACEMENT_3D('',#18527,#14940,#14941);
#13582=AXIS2_PLACEMENT_3D('',#18530,#14943,#14944);
#13583=AXIS2_PLACEMENT_3D('',#18531,#14945,#14946);
#13584=AXIS2_PLACEMENT_3D('',#18533,#14947,#14948);
#13585=AXIS2_PLACEMENT_3D('',#18536,#14950,#14951);
#13586=AXIS2_PLACEMENT_3D('',#18537,#14952,#14953);
#13587=AXIS2_PLACEMENT_3D('',#18539,#14954,#14955);
#13588=AXIS2_PLACEMENT_3D('',#18542,#14957,#14958);
#13589=AXIS2_PLACEMENT_3D('',#18543,#14959,#14960);
#13590=AXIS2_PLACEMENT_3D('',#18545,#14961,#14962);
#13591=AXIS2_PLACEMENT_3D('',#18548,#14964,#14965);
#13592=AXIS2_PLACEMENT_3D('',#18549,#14966,#14967);
#13593=AXIS2_PLACEMENT_3D('',#18551,#14968,#14969);
#13594=AXIS2_PLACEMENT_3D('',#18554,#14971,#14972);
#13595=AXIS2_PLACEMENT_3D('',#18555,#14973,#14974);
#13596=AXIS2_PLACEMENT_3D('',#18557,#14975,#14976);
#13597=AXIS2_PLACEMENT_3D('',#18560,#14978,#14979);
#13598=AXIS2_PLACEMENT_3D('',#18561,#14980,#14981);
#13599=AXIS2_PLACEMENT_3D('',#18563,#14982,#14983);
#13600=AXIS2_PLACEMENT_3D('',#18566,#14985,#14986);
#13601=AXIS2_PLACEMENT_3D('',#18567,#14987,#14988);
#13602=AXIS2_PLACEMENT_3D('',#18569,#14989,#14990);
#13603=AXIS2_PLACEMENT_3D('',#18572,#14992,#14993);
#13604=AXIS2_PLACEMENT_3D('',#18573,#14994,#14995);
#13605=AXIS2_PLACEMENT_3D('',#18575,#14996,#14997);
#13606=AXIS2_PLACEMENT_3D('',#18578,#14999,#15000);
#13607=AXIS2_PLACEMENT_3D('',#18579,#15001,#15002);
#13608=AXIS2_PLACEMENT_3D('',#18581,#15003,#15004);
#13609=AXIS2_PLACEMENT_3D('',#18584,#15006,#15007);
#13610=AXIS2_PLACEMENT_3D('',#18585,#15008,#15009);
#13611=AXIS2_PLACEMENT_3D('',#18594,#15014,#15015);
#13612=AXIS2_PLACEMENT_3D('',#18600,#15019,#15020);
#13613=AXIS2_PLACEMENT_3D('',#18606,#15024,#15025);
#13614=AXIS2_PLACEMENT_3D('',#18609,#15028,#15029);
#13615=AXIS2_PLACEMENT_3D('',#18610,#15030,#15031);
#13616=AXIS2_PLACEMENT_3D('',#18611,#15032,#15033);
#13617=AXIS2_PLACEMENT_3D('',#18612,#15034,#15035);
#13618=AXIS2_PLACEMENT_3D('',#18614,#15036,#15037);
#13619=AXIS2_PLACEMENT_3D('',#18617,#15039,#15040);
#13620=AXIS2_PLACEMENT_3D('',#18618,#15041,#15042);
#13621=AXIS2_PLACEMENT_3D('',#18620,#15043,#15044);
#13622=AXIS2_PLACEMENT_3D('',#18623,#15046,#15047);
#13623=AXIS2_PLACEMENT_3D('',#18624,#15048,#15049);
#13624=AXIS2_PLACEMENT_3D('',#18626,#15050,#15051);
#13625=AXIS2_PLACEMENT_3D('',#18629,#15053,#15054);
#13626=AXIS2_PLACEMENT_3D('',#18630,#15055,#15056);
#13627=AXIS2_PLACEMENT_3D('',#18632,#15057,#15058);
#13628=AXIS2_PLACEMENT_3D('',#18635,#15060,#15061);
#13629=AXIS2_PLACEMENT_3D('',#18636,#15062,#15063);
#13630=AXIS2_PLACEMENT_3D('',#18638,#15064,#15065);
#13631=AXIS2_PLACEMENT_3D('',#18641,#15067,#15068);
#13632=AXIS2_PLACEMENT_3D('',#18642,#15069,#15070);
#13633=AXIS2_PLACEMENT_3D('',#18644,#15071,#15072);
#13634=AXIS2_PLACEMENT_3D('',#18645,#15073,#15074);
#13635=AXIS2_PLACEMENT_3D('',#18647,#15075,#15076);
#13636=AXIS2_PLACEMENT_3D('',#18650,#15078,#15079);
#13637=AXIS2_PLACEMENT_3D('',#18651,#15080,#15081);
#13638=AXIS2_PLACEMENT_3D('',#18653,#15082,#15083);
#13639=AXIS2_PLACEMENT_3D('',#18654,#15084,#15085);
#13640=AXIS2_PLACEMENT_3D('',#18656,#15086,#15087);
#13641=AXIS2_PLACEMENT_3D('',#18659,#15089,#15090);
#13642=AXIS2_PLACEMENT_3D('',#18660,#15091,#15092);
#13643=AXIS2_PLACEMENT_3D('',#18662,#15093,#15094);
#13644=AXIS2_PLACEMENT_3D('',#18663,#15095,#15096);
#13645=AXIS2_PLACEMENT_3D('',#18665,#15097,#15098);
#13646=AXIS2_PLACEMENT_3D('',#18668,#15100,#15101);
#13647=AXIS2_PLACEMENT_3D('',#18669,#15102,#15103);
#13648=AXIS2_PLACEMENT_3D('',#18671,#15104,#15105);
#13649=AXIS2_PLACEMENT_3D('',#18672,#15106,#15107);
#13650=AXIS2_PLACEMENT_3D('',#18674,#15108,#15109);
#13651=AXIS2_PLACEMENT_3D('',#18676,#15111,#15112);
#13652=AXIS2_PLACEMENT_3D('',#18678,#15113,#15114);
#13653=AXIS2_PLACEMENT_3D('',#18680,#15116,#15117);
#13654=AXIS2_PLACEMENT_3D('',#18682,#15118,#15119);
#13655=AXIS2_PLACEMENT_3D('',#18684,#15121,#15122);
#13656=AXIS2_PLACEMENT_3D('',#18686,#15123,#15124);
#13657=AXIS2_PLACEMENT_3D('',#18688,#15126,#15127);
#13658=AXIS2_PLACEMENT_3D('',#18697,#15132,#15133);
#13659=AXIS2_PLACEMENT_3D('',#18703,#15137,#15138);
#13660=AXIS2_PLACEMENT_3D('',#18709,#15142,#15143);
#13661=AXIS2_PLACEMENT_3D('',#18712,#15146,#15147);
#13662=AXIS2_PLACEMENT_3D('',#18713,#15148,#15149);
#13663=AXIS2_PLACEMENT_3D('',#18714,#15150,#15151);
#13664=AXIS2_PLACEMENT_3D('',#18715,#15152,#15153);
#13665=AXIS2_PLACEMENT_3D('',#18717,#15154,#15155);
#13666=AXIS2_PLACEMENT_3D('',#18720,#15157,#15158);
#13667=AXIS2_PLACEMENT_3D('',#18721,#15159,#15160);
#13668=AXIS2_PLACEMENT_3D('',#18723,#15161,#15162);
#13669=AXIS2_PLACEMENT_3D('',#18726,#15164,#15165);
#13670=AXIS2_PLACEMENT_3D('',#18727,#15166,#15167);
#13671=AXIS2_PLACEMENT_3D('',#18729,#15168,#15169);
#13672=AXIS2_PLACEMENT_3D('',#18732,#15171,#15172);
#13673=AXIS2_PLACEMENT_3D('',#18733,#15173,#15174);
#13674=AXIS2_PLACEMENT_3D('',#18735,#15175,#15176);
#13675=AXIS2_PLACEMENT_3D('',#18738,#15178,#15179);
#13676=AXIS2_PLACEMENT_3D('',#18739,#15180,#15181);
#13677=AXIS2_PLACEMENT_3D('',#18741,#15182,#15183);
#13678=AXIS2_PLACEMENT_3D('',#18742,#15184,#15185);
#13679=AXIS2_PLACEMENT_3D('',#18745,#15187,#15188);
#13680=AXIS2_PLACEMENT_3D('',#18746,#15189,#15190);
#13681=AXIS2_PLACEMENT_3D('',#18748,#15191,#15192);
#13682=AXIS2_PLACEMENT_3D('',#18751,#15194,#15195);
#13683=AXIS2_PLACEMENT_3D('',#18752,#15196,#15197);
#13684=AXIS2_PLACEMENT_3D('',#18753,#15198,#15199);
#13685=AXIS2_PLACEMENT_3D('',#18755,#15200,#15201);
#13686=AXIS2_PLACEMENT_3D('',#18758,#15203,#15204);
#13687=AXIS2_PLACEMENT_3D('',#18759,#15205,#15206);
#13688=AXIS2_PLACEMENT_3D('',#18760,#15207,#15208);
#13689=AXIS2_PLACEMENT_3D('',#18769,#15213,#15214);
#13690=AXIS2_PLACEMENT_3D('',#18775,#15218,#15219);
#13691=AXIS2_PLACEMENT_3D('',#18781,#15223,#15224);
#13692=AXIS2_PLACEMENT_3D('',#18784,#15227,#15228);
#13693=AXIS2_PLACEMENT_3D('',#18785,#15229,#15230);
#13694=AXIS2_PLACEMENT_3D('',#18786,#15231,#15232);
#13695=AXIS2_PLACEMENT_3D('',#18787,#15233,#15234);
#13696=AXIS2_PLACEMENT_3D('',#18789,#15235,#15236);
#13697=AXIS2_PLACEMENT_3D('',#18792,#15238,#15239);
#13698=AXIS2_PLACEMENT_3D('',#18793,#15240,#15241);
#13699=AXIS2_PLACEMENT_3D('',#18795,#15242,#15243);
#13700=AXIS2_PLACEMENT_3D('',#18798,#15245,#15246);
#13701=AXIS2_PLACEMENT_3D('',#18799,#15247,#15248);
#13702=AXIS2_PLACEMENT_3D('',#18801,#15249,#15250);
#13703=AXIS2_PLACEMENT_3D('',#18804,#15252,#15253);
#13704=AXIS2_PLACEMENT_3D('',#18805,#15254,#15255);
#13705=AXIS2_PLACEMENT_3D('',#18807,#15256,#15257);
#13706=AXIS2_PLACEMENT_3D('',#18810,#15259,#15260);
#13707=AXIS2_PLACEMENT_3D('',#18811,#15261,#15262);
#13708=AXIS2_PLACEMENT_3D('',#18813,#15263,#15264);
#13709=AXIS2_PLACEMENT_3D('',#18814,#15265,#15266);
#13710=AXIS2_PLACEMENT_3D('',#18817,#15268,#15269);
#13711=AXIS2_PLACEMENT_3D('',#18818,#15270,#15271);
#13712=AXIS2_PLACEMENT_3D('',#18820,#15272,#15273);
#13713=AXIS2_PLACEMENT_3D('',#18823,#15275,#15276);
#13714=AXIS2_PLACEMENT_3D('',#18824,#15277,#15278);
#13715=AXIS2_PLACEMENT_3D('',#18825,#15279,#15280);
#13716=AXIS2_PLACEMENT_3D('',#18826,#15281,#15282);
#13717=AXIS2_PLACEMENT_3D('',#18827,#15283,#15284);
#13718=AXIS2_PLACEMENT_3D('',#18829,#15285,#15286);
#13719=AXIS2_PLACEMENT_3D('',#18832,#15288,#15289);
#13720=AXIS2_PLACEMENT_3D('',#18833,#15290,#15291);
#13721=AXIS2_PLACEMENT_3D('',#18835,#15292,#15293);
#13722=AXIS2_PLACEMENT_3D('',#18838,#15295,#15296);
#13723=AXIS2_PLACEMENT_3D('',#18839,#15297,#15298);
#13724=AXIS2_PLACEMENT_3D('',#18841,#15299,#15300);
#13725=AXIS2_PLACEMENT_3D('',#18844,#15302,#15303);
#13726=AXIS2_PLACEMENT_3D('',#18845,#15304,#15305);
#13727=AXIS2_PLACEMENT_3D('',#18847,#15306,#15307);
#13728=AXIS2_PLACEMENT_3D('',#18850,#15309,#15310);
#13729=AXIS2_PLACEMENT_3D('',#18851,#15311,#15312);
#13730=AXIS2_PLACEMENT_3D('',#18853,#15313,#15314);
#13731=AXIS2_PLACEMENT_3D('',#18854,#15315,#15316);
#13732=AXIS2_PLACEMENT_3D('',#18856,#15317,#15318);
#13733=AXIS2_PLACEMENT_3D('',#18858,#15320,#15321);
#13734=AXIS2_PLACEMENT_3D('',#18860,#15322,#15323);
#13735=AXIS2_PLACEMENT_3D('',#18863,#15325,#15326);
#13736=AXIS2_PLACEMENT_3D('',#18864,#15327,#15328);
#13737=AXIS2_PLACEMENT_3D('',#18865,#15329,#15330);
#13738=AXIS2_PLACEMENT_3D('',#18867,#15331,#15332);
#13739=AXIS2_PLACEMENT_3D('',#18870,#15334,#15335);
#13740=AXIS2_PLACEMENT_3D('',#18871,#15336,#15337);
#13741=AXIS2_PLACEMENT_3D('',#18872,#15338,#15339);
#13742=AXIS2_PLACEMENT_3D('',#18881,#15344,#15345);
#13743=AXIS2_PLACEMENT_3D('',#18887,#15349,#15350);
#13744=AXIS2_PLACEMENT_3D('',#18893,#15354,#15355);
#13745=AXIS2_PLACEMENT_3D('',#18896,#15358,#15359);
#13746=AXIS2_PLACEMENT_3D('',#18897,#15360,#15361);
#13747=AXIS2_PLACEMENT_3D('',#18898,#15362,#15363);
#13748=AXIS2_PLACEMENT_3D('',#18899,#15364,#15365);
#13749=AXIS2_PLACEMENT_3D('',#18908,#15370,#15371);
#13750=AXIS2_PLACEMENT_3D('',#18909,#15372,#15373);
#13751=AXIS2_PLACEMENT_3D('',#18911,#15374,#15375);
#13752=AXIS2_PLACEMENT_3D('',#18913,#15376,#15377);
#13753=AXIS2_PLACEMENT_3D('',#18915,#15378,#15379);
#13754=AXIS2_PLACEMENT_3D('',#18917,#15380,#15381);
#13755=AXIS2_PLACEMENT_3D('',#18918,#15382,#15383);
#13756=AXIS2_PLACEMENT_3D('',#18919,#15384,#15385);
#13757=AXIS2_PLACEMENT_3D('',#18920,#15386,#15387);
#13758=AXIS2_PLACEMENT_3D('',#18923,#15389,#15390);
#13759=AXIS2_PLACEMENT_3D('',#18924,#15391,#15392);
#13760=AXIS2_PLACEMENT_3D('',#18927,#15394,#15395);
#13761=AXIS2_PLACEMENT_3D('',#18928,#15396,#15397);
#13762=AXIS2_PLACEMENT_3D('',#18931,#15399,#15400);
#13763=AXIS2_PLACEMENT_3D('',#18932,#15401,#15402);
#13764=AXIS2_PLACEMENT_3D('',#18935,#15404,#15405);
#13765=AXIS2_PLACEMENT_3D('',#18936,#15406,#15407);
#13766=AXIS2_PLACEMENT_3D('',#18938,#15408,#15409);
#13767=AXIS2_PLACEMENT_3D('',#18939,#15410,#15411);
#13768=AXIS2_PLACEMENT_3D('',#18941,#15412,#15413);
#13769=AXIS2_PLACEMENT_3D('',#18943,#15415,#15416);
#13770=AXIS2_PLACEMENT_3D('',#18944,#15417,#15418);
#13771=AXIS2_PLACEMENT_3D('',#18945,#15419,#15420);
#13772=AXIS2_PLACEMENT_3D('',#18950,#15422,#15423);
#13773=AXIS2_PLACEMENT_3D('',#18951,#15424,#15425);
#13774=AXIS2_PLACEMENT_3D('',#18953,#15426,#15427);
#13775=AXIS2_PLACEMENT_3D('',#18954,#15428,#15429);
#13776=AXIS2_PLACEMENT_3D('',#18958,#15431,#15432);
#13777=AXIS2_PLACEMENT_3D('',#18962,#15435,#15436);
#13778=AXIS2_PLACEMENT_3D('',#18963,#15437,#15438);
#13779=AXIS2_PLACEMENT_3D('',#18968,#15440,#15441);
#13780=AXIS2_PLACEMENT_3D('',#18969,#15442,#15443);
#13781=AXIS2_PLACEMENT_3D('',#18971,#15444,#15445);
#13782=AXIS2_PLACEMENT_3D('',#18972,#15446,#15447);
#13783=AXIS2_PLACEMENT_3D('',#18976,#15449,#15450);
#13784=AXIS2_PLACEMENT_3D('',#18980,#15453,#15454);
#13785=AXIS2_PLACEMENT_3D('',#18981,#15455,#15456);
#13786=AXIS2_PLACEMENT_3D('',#18991,#15462,#15463);
#13787=AXIS2_PLACEMENT_3D('',#19001,#15469,#15470);
#13788=AXIS2_PLACEMENT_3D('',#19003,#15471,#15472);
#13789=AXIS2_PLACEMENT_3D('',#19005,#15474,#15475);
#13790=AXIS2_PLACEMENT_3D('',#19007,#15476,#15477);
#13791=AXIS2_PLACEMENT_3D('',#19009,#15479,#15480);
#13792=AXIS2_PLACEMENT_3D('',#19012,#15483,#15484);
#13793=AXIS2_PLACEMENT_3D('',#19022,#15490,#15491);
#13794=AXIS2_PLACEMENT_3D('',#19026,#15494,#15495);
#13795=AXIS2_PLACEMENT_3D('',#19030,#15498,#15499);
#13796=AXIS2_PLACEMENT_3D('',#19036,#15503,#15504);
#13797=AXIS2_PLACEMENT_3D('',#19039,#15507,#15508);
#13798=AXIS2_PLACEMENT_3D('',#19040,#15509,#15510);
#13799=AXIS2_PLACEMENT_3D('',#19041,#15511,#15512);
#13800=AXIS2_PLACEMENT_3D('',#19042,#15513,#15514);
#13801=AXIS2_PLACEMENT_3D('',#19047,#15516,#15517);
#13802=AXIS2_PLACEMENT_3D('',#19048,#15518,#15519);
#13803=AXIS2_PLACEMENT_3D('',#19050,#15520,#15521);
#13804=AXIS2_PLACEMENT_3D('',#19051,#15522,#15523);
#13805=AXIS2_PLACEMENT_3D('',#19055,#15525,#15526);
#13806=AXIS2_PLACEMENT_3D('',#19059,#15529,#15530);
#13807=AXIS2_PLACEMENT_3D('',#19060,#15531,#15532);
#13808=AXIS2_PLACEMENT_3D('',#19065,#15534,#15535);
#13809=AXIS2_PLACEMENT_3D('',#19066,#15536,#15537);
#13810=AXIS2_PLACEMENT_3D('',#19068,#15538,#15539);
#13811=AXIS2_PLACEMENT_3D('',#19069,#15540,#15541);
#13812=AXIS2_PLACEMENT_3D('',#19073,#15543,#15544);
#13813=AXIS2_PLACEMENT_3D('',#19077,#15547,#15548);
#13814=AXIS2_PLACEMENT_3D('',#19078,#15549,#15550);
#13815=AXIS2_PLACEMENT_3D('',#19088,#15556,#15557);
#13816=AXIS2_PLACEMENT_3D('',#19098,#15563,#15564);
#13817=AXIS2_PLACEMENT_3D('',#19100,#15565,#15566);
#13818=AXIS2_PLACEMENT_3D('',#19102,#15568,#15569);
#13819=AXIS2_PLACEMENT_3D('',#19104,#15570,#15571);
#13820=AXIS2_PLACEMENT_3D('',#19106,#15573,#15574);
#13821=AXIS2_PLACEMENT_3D('',#19109,#15577,#15578);
#13822=AXIS2_PLACEMENT_3D('',#19119,#15584,#15585);
#13823=AXIS2_PLACEMENT_3D('',#19123,#15588,#15589);
#13824=AXIS2_PLACEMENT_3D('',#19127,#15592,#15593);
#13825=AXIS2_PLACEMENT_3D('',#19133,#15597,#15598);
#13826=AXIS2_PLACEMENT_3D('',#19136,#15601,#15602);
#13827=AXIS2_PLACEMENT_3D('',#19137,#15603,#15604);
#13828=AXIS2_PLACEMENT_3D('',#19138,#15605,#15606);
#13829=AXIS2_PLACEMENT_3D('',#19139,#15607,#15608);
#13830=AXIS2_PLACEMENT_3D('',#19141,#15609,#15610);
#13831=AXIS2_PLACEMENT_3D('',#19144,#15612,#15613);
#13832=AXIS2_PLACEMENT_3D('',#19145,#15614,#15615);
#13833=AXIS2_PLACEMENT_3D('',#19147,#15616,#15617);
#13834=AXIS2_PLACEMENT_3D('',#19148,#15618,#15619);
#13835=AXIS2_PLACEMENT_3D('',#19150,#15620,#15621);
#13836=AXIS2_PLACEMENT_3D('',#19153,#15623,#15624);
#13837=AXIS2_PLACEMENT_3D('',#19154,#15625,#15626);
#13838=AXIS2_PLACEMENT_3D('',#19156,#15627,#15628);
#13839=AXIS2_PLACEMENT_3D('',#19157,#15629,#15630);
#13840=AXIS2_PLACEMENT_3D('',#19159,#15631,#15632);
#13841=AXIS2_PLACEMENT_3D('',#19162,#15634,#15635);
#13842=AXIS2_PLACEMENT_3D('',#19163,#15636,#15637);
#13843=AXIS2_PLACEMENT_3D('',#19165,#15638,#15639);
#13844=AXIS2_PLACEMENT_3D('',#19166,#15640,#15641);
#13845=AXIS2_PLACEMENT_3D('',#19168,#15642,#15643);
#13846=AXIS2_PLACEMENT_3D('',#19171,#15645,#15646);
#13847=AXIS2_PLACEMENT_3D('',#19172,#15647,#15648);
#13848=AXIS2_PLACEMENT_3D('',#19174,#15649,#15650);
#13849=AXIS2_PLACEMENT_3D('',#19175,#15651,#15652);
#13850=AXIS2_PLACEMENT_3D('',#19177,#15653,#15654);
#13851=AXIS2_PLACEMENT_3D('',#19179,#15656,#15657);
#13852=AXIS2_PLACEMENT_3D('',#19181,#15658,#15659);
#13853=AXIS2_PLACEMENT_3D('',#19183,#15661,#15662);
#13854=AXIS2_PLACEMENT_3D('',#19185,#15663,#15664);
#13855=AXIS2_PLACEMENT_3D('',#19187,#15666,#15667);
#13856=AXIS2_PLACEMENT_3D('',#19189,#15668,#15669);
#13857=AXIS2_PLACEMENT_3D('',#19191,#15671,#15672);
#13858=AXIS2_PLACEMENT_3D('',#19200,#15677,#15678);
#13859=AXIS2_PLACEMENT_3D('',#19206,#15682,#15683);
#13860=AXIS2_PLACEMENT_3D('',#19212,#15687,#15688);
#13861=AXIS2_PLACEMENT_3D('',#19218,#15692,#15693);
#13862=AXIS2_PLACEMENT_3D('',#19224,#15697,#15698);
#13863=AXIS2_PLACEMENT_3D('',#19230,#15702,#15703);
#13864=AXIS2_PLACEMENT_3D('',#19236,#15707,#15708);
#13865=AXIS2_PLACEMENT_3D('',#19242,#15712,#15713);
#13866=AXIS2_PLACEMENT_3D('',#19248,#15717,#15718);
#13867=AXIS2_PLACEMENT_3D('',#19254,#15722,#15723);
#13868=AXIS2_PLACEMENT_3D('',#19260,#15727,#15728);
#13869=AXIS2_PLACEMENT_3D('',#19263,#15731,#15732);
#13870=AXIS2_PLACEMENT_3D('',#19264,#15733,#15734);
#13871=AXIS2_PLACEMENT_3D('',#19265,#15735,#15736);
#13872=AXIS2_PLACEMENT_3D('',#19266,#15737,#15738);
#13873=AXIS2_PLACEMENT_3D('',#19267,#15739,#15740);
#13874=AXIS2_PLACEMENT_3D('',#19270,#15741,#15742);
#13875=AXIS2_PLACEMENT_3D('',#19271,#15743,#15744);
#13876=AXIS2_PLACEMENT_3D('',#19273,#15745,#15746);
#13877=AXIS2_PLACEMENT_3D('',#19275,#15747,#15748);
#13878=AXIS2_PLACEMENT_3D('',#19276,#15749,#15750);
#13879=AXIS2_PLACEMENT_3D('',#19277,#15751,#15752);
#13880=AXIS2_PLACEMENT_3D('',#19280,#15754,#15755);
#13881=AXIS2_PLACEMENT_3D('',#19281,#15756,#15757);
#13882=AXIS2_PLACEMENT_3D('',#19283,#15758,#15759);
#13883=AXIS2_PLACEMENT_3D('',#19286,#15761,#15762);
#13884=AXIS2_PLACEMENT_3D('',#19287,#15763,#15764);
#13885=AXIS2_PLACEMENT_3D('',#19290,#15766,#15767);
#13886=AXIS2_PLACEMENT_3D('',#19291,#15768,#15769);
#13887=AXIS2_PLACEMENT_3D('',#19292,#15770,#15771);
#13888=AXIS2_PLACEMENT_3D('',#19294,#15772,#15773);
#13889=AXIS2_PLACEMENT_3D('',#19296,#15775,#15776);
#13890=AXIS2_PLACEMENT_3D('',#19298,#15777,#15778);
#13891=AXIS2_PLACEMENT_3D('',#19299,#15779,#15780);
#13892=AXIS2_PLACEMENT_3D('',#19301,#15782,#15783);
#13893=AXIS2_PLACEMENT_3D('',#19302,#15784,#15785);
#13894=AXIS2_PLACEMENT_3D('',#19305,#15786,#15787);
#13895=AXIS2_PLACEMENT_3D('',#19306,#15788,#15789);
#13896=AXIS2_PLACEMENT_3D('',#19308,#15790,#15791);
#13897=AXIS2_PLACEMENT_3D('',#19310,#15792,#15793);
#13898=AXIS2_PLACEMENT_3D('',#19311,#15794,#15795);
#13899=AXIS2_PLACEMENT_3D('',#19312,#15796,#15797);
#13900=AXIS2_PLACEMENT_3D('',#19314,#15798,#15799);
#13901=AXIS2_PLACEMENT_3D('',#19316,#15801,#15802);
#13902=AXIS2_PLACEMENT_3D('',#19318,#15803,#15804);
#13903=AXIS2_PLACEMENT_3D('',#19320,#15805,#15806);
#13904=AXIS2_PLACEMENT_3D('',#19321,#15807,#15808);
#13905=AXIS2_PLACEMENT_3D('',#19323,#15809,#15810);
#13906=AXIS2_PLACEMENT_3D('',#19325,#15812,#15813);
#13907=AXIS2_PLACEMENT_3D('',#19327,#15814,#15815);
#13908=AXIS2_PLACEMENT_3D('',#19329,#15817,#15818);
#13909=AXIS2_PLACEMENT_3D('',#19331,#15819,#15820);
#13910=AXIS2_PLACEMENT_3D('',#19333,#15822,#15823);
#13911=AXIS2_PLACEMENT_3D('',#19334,#15824,#15825);
#13912=AXIS2_PLACEMENT_3D('',#19336,#15827,#15828);
#13913=AXIS2_PLACEMENT_3D('',#19337,#15829,#15830);
#13914=AXIS2_PLACEMENT_3D('',#19340,#15831,#15832);
#13915=AXIS2_PLACEMENT_3D('',#19341,#15833,#15834);
#13916=AXIS2_PLACEMENT_3D('',#19344,#15835,#15836);
#13917=AXIS2_PLACEMENT_3D('',#19345,#15837,#15838);
#13918=AXIS2_PLACEMENT_3D('',#19348,#15839,#15840);
#13919=AXIS2_PLACEMENT_3D('',#19349,#15841,#15842);
#13920=AXIS2_PLACEMENT_3D('',#19352,#15843,#15844);
#13921=AXIS2_PLACEMENT_3D('',#19353,#15845,#15846);
#13922=AXIS2_PLACEMENT_3D('',#19356,#15847,#15848);
#13923=AXIS2_PLACEMENT_3D('',#19357,#15849,#15850);
#13924=AXIS2_PLACEMENT_3D('',#19360,#15851,#15852);
#13925=AXIS2_PLACEMENT_3D('',#19361,#15853,#15854);
#13926=AXIS2_PLACEMENT_3D('',#19364,#15855,#15856);
#13927=AXIS2_PLACEMENT_3D('',#19365,#15857,#15858);
#13928=AXIS2_PLACEMENT_3D('',#19366,#15859,#15860);
#13929=AXIS2_PLACEMENT_3D('',#19392,#15861,#15862);
#13930=AXIS2_PLACEMENT_3D('',#19416,#15863,#15864);
#13931=AXIS2_PLACEMENT_3D('',#19417,#15865,#15866);
#13932=AXIS2_PLACEMENT_3D('',#19419,#15867,#15868);
#13933=AXIS2_PLACEMENT_3D('',#19444,#15869,#15870);
#13934=AXIS2_PLACEMENT_3D('',#19469,#15871,#15872);
#13935=AXIS2_PLACEMENT_3D('',#19472,#15874,#15875);
#13936=AXIS2_PLACEMENT_3D('',#19474,#15876,#15877);
#13937=AXIS2_PLACEMENT_3D('',#19499,#15878,#15879);
#13938=AXIS2_PLACEMENT_3D('',#19524,#15880,#15881);
#13939=AXIS2_PLACEMENT_3D('',#19549,#15882,#15883);
#13940=AXIS2_PLACEMENT_3D('',#19573,#15884,#15885);
#13941=AXIS2_PLACEMENT_3D('',#19574,#15886,#15887);
#13942=AXIS2_PLACEMENT_3D('',#19576,#15888,#15889);
#13943=AXIS2_PLACEMENT_3D('',#19577,#15890,#15891);
#13944=AXIS2_PLACEMENT_3D('',#19578,#15892,#15893);
#13945=AXIS2_PLACEMENT_3D('',#19602,#15894,#15895);
#13946=AXIS2_PLACEMENT_3D('',#19603,#15896,#15897);
#13947=AXIS2_PLACEMENT_3D('',#19605,#15898,#15899);
#13948=AXIS2_PLACEMENT_3D('',#19606,#15900,#15901);
#13949=AXIS2_PLACEMENT_3D('',#19607,#15902,#15903);
#13950=AXIS2_PLACEMENT_3D('',#19631,#15904,#15905);
#13951=AXIS2_PLACEMENT_3D('',#19632,#15906,#15907);
#13952=AXIS2_PLACEMENT_3D('',#19634,#15908,#15909);
#13953=AXIS2_PLACEMENT_3D('',#19636,#15910,#15911);
#13954=AXIS2_PLACEMENT_3D('',#19637,#15912,#15913);
#13955=AXIS2_PLACEMENT_3D('',#19638,#15914,#15915);
#13956=AXIS2_PLACEMENT_3D('',#19662,#15916,#15917);
#13957=AXIS2_PLACEMENT_3D('',#19663,#15918,#15919);
#13958=AXIS2_PLACEMENT_3D('',#19665,#15920,#15921);
#13959=AXIS2_PLACEMENT_3D('',#19666,#15922,#15923);
#13960=AXIS2_PLACEMENT_3D('',#19667,#15924,#15925);
#13961=AXIS2_PLACEMENT_3D('',#19691,#15926,#15927);
#13962=AXIS2_PLACEMENT_3D('',#19692,#15928,#15929);
#13963=AXIS2_PLACEMENT_3D('',#19694,#15930,#15931);
#13964=AXIS2_PLACEMENT_3D('',#19695,#15932,#15933);
#13965=AXIS2_PLACEMENT_3D('',#19696,#15934,#15935);
#13966=AXIS2_PLACEMENT_3D('',#19720,#15936,#15937);
#13967=AXIS2_PLACEMENT_3D('',#19721,#15938,#15939);
#13968=AXIS2_PLACEMENT_3D('',#19723,#15940,#15941);
#13969=AXIS2_PLACEMENT_3D('',#19726,#15943,#15944);
#13970=AXIS2_PLACEMENT_3D('',#19750,#15945,#15946);
#13971=AXIS2_PLACEMENT_3D('',#19751,#15947,#15948);
#13972=AXIS2_PLACEMENT_3D('',#19752,#15949,#15950);
#13973=AXIS2_PLACEMENT_3D('',#19753,#15951,#15952);
#13974=AXIS2_PLACEMENT_3D('',#19754,#15953,#15954);
#13975=AXIS2_PLACEMENT_3D('',#19755,#15955,#15956);
#13976=AXIS2_PLACEMENT_3D('',#19756,#15957,#15958);
#13977=AXIS2_PLACEMENT_3D('',#19757,#15959,#15960);
#13978=AXIS2_PLACEMENT_3D('',#19758,#15961,#15962);
#13979=AXIS2_PLACEMENT_3D('',#19760,#15963,#15964);
#13980=AXIS2_PLACEMENT_3D('',#19762,#15965,#15966);
#13981=AXIS2_PLACEMENT_3D('',#19763,#15967,#15968);
#13982=AXIS2_PLACEMENT_3D('',#19765,#15969,#15970);
#13983=AXIS2_PLACEMENT_3D('',#19767,#15972,#15973);
#13984=AXIS2_PLACEMENT_3D('',#19769,#15974,#15975);
#13985=AXIS2_PLACEMENT_3D('',#19770,#15976,#15977);
#13986=AXIS2_PLACEMENT_3D('',#19772,#15979,#15980);
#13987=AXIS2_PLACEMENT_3D('',#19774,#15981,#15982);
#13988=AXIS2_PLACEMENT_3D('',#19776,#15983,#15984);
#13989=AXIS2_PLACEMENT_3D('',#19777,#15985,#15986);
#13990=AXIS2_PLACEMENT_3D('',#19779,#15987,#15988);
#13991=AXIS2_PLACEMENT_3D('',#19781,#15990,#15991);
#13992=AXIS2_PLACEMENT_3D('',#19783,#15992,#15993);
#13993=AXIS2_PLACEMENT_3D('',#19784,#15994,#15995);
#13994=AXIS2_PLACEMENT_3D('',#19786,#15997,#15998);
#13995=AXIS2_PLACEMENT_3D('',#19787,#15999,#16000);
#13996=AXIS2_PLACEMENT_3D('',#19788,#16001,#16002);
#13997=AXIS2_PLACEMENT_3D('',#19789,#16003,#16004);
#13998=AXIS2_PLACEMENT_3D('',#19790,#16005,#16006);
#13999=AXIS2_PLACEMENT_3D('',#19791,#16007,#16008);
#14000=AXIS2_PLACEMENT_3D('',#19792,#16009,#16010);
#14001=AXIS2_PLACEMENT_3D('',#19793,#16011,#16012);
#14002=AXIS2_PLACEMENT_3D('',#19796,#16013,#16014);
#14003=AXIS2_PLACEMENT_3D('',#19797,#16015,#16016);
#14004=AXIS2_PLACEMENT_3D('',#19799,#16017,#16018);
#14005=AXIS2_PLACEMENT_3D('',#19801,#16019,#16020);
#14006=AXIS2_PLACEMENT_3D('',#19802,#16021,#16022);
#14007=AXIS2_PLACEMENT_3D('',#19803,#16023,#16024);
#14008=AXIS2_PLACEMENT_3D('',#19806,#16026,#16027);
#14009=AXIS2_PLACEMENT_3D('',#19807,#16028,#16029);
#14010=AXIS2_PLACEMENT_3D('',#19809,#16030,#16031);
#14011=AXIS2_PLACEMENT_3D('',#19812,#16033,#16034);
#14012=AXIS2_PLACEMENT_3D('',#19813,#16035,#16036);
#14013=AXIS2_PLACEMENT_3D('',#19816,#16038,#16039);
#14014=AXIS2_PLACEMENT_3D('',#19817,#16040,#16041);
#14015=AXIS2_PLACEMENT_3D('',#19818,#16042,#16043);
#14016=AXIS2_PLACEMENT_3D('',#19820,#16044,#16045);
#14017=AXIS2_PLACEMENT_3D('',#19822,#16047,#16048);
#14018=AXIS2_PLACEMENT_3D('',#19824,#16049,#16050);
#14019=AXIS2_PLACEMENT_3D('',#19825,#16051,#16052);
#14020=AXIS2_PLACEMENT_3D('',#19827,#16054,#16055);
#14021=AXIS2_PLACEMENT_3D('',#19828,#16056,#16057);
#14022=AXIS2_PLACEMENT_3D('',#19831,#16058,#16059);
#14023=AXIS2_PLACEMENT_3D('',#19832,#16060,#16061);
#14024=AXIS2_PLACEMENT_3D('',#19834,#16062,#16063);
#14025=AXIS2_PLACEMENT_3D('',#19836,#16064,#16065);
#14026=AXIS2_PLACEMENT_3D('',#19837,#16066,#16067);
#14027=AXIS2_PLACEMENT_3D('',#19838,#16068,#16069);
#14028=AXIS2_PLACEMENT_3D('',#19840,#16070,#16071);
#14029=AXIS2_PLACEMENT_3D('',#19842,#16073,#16074);
#14030=AXIS2_PLACEMENT_3D('',#19844,#16075,#16076);
#14031=AXIS2_PLACEMENT_3D('',#19846,#16077,#16078);
#14032=AXIS2_PLACEMENT_3D('',#19847,#16079,#16080);
#14033=AXIS2_PLACEMENT_3D('',#19849,#16081,#16082);
#14034=AXIS2_PLACEMENT_3D('',#19851,#16084,#16085);
#14035=AXIS2_PLACEMENT_3D('',#19853,#16086,#16087);
#14036=AXIS2_PLACEMENT_3D('',#19855,#16089,#16090);
#14037=AXIS2_PLACEMENT_3D('',#19857,#16091,#16092);
#14038=AXIS2_PLACEMENT_3D('',#19859,#16094,#16095);
#14039=AXIS2_PLACEMENT_3D('',#19860,#16096,#16097);
#14040=AXIS2_PLACEMENT_3D('',#19862,#16099,#16100);
#14041=AXIS2_PLACEMENT_3D('',#19863,#16101,#16102);
#14042=AXIS2_PLACEMENT_3D('',#19866,#16103,#16104);
#14043=AXIS2_PLACEMENT_3D('',#19867,#16105,#16106);
#14044=AXIS2_PLACEMENT_3D('',#19870,#16107,#16108);
#14045=AXIS2_PLACEMENT_3D('',#19871,#16109,#16110);
#14046=AXIS2_PLACEMENT_3D('',#19874,#16111,#16112);
#14047=AXIS2_PLACEMENT_3D('',#19875,#16113,#16114);
#14048=AXIS2_PLACEMENT_3D('',#19878,#16115,#16116);
#14049=AXIS2_PLACEMENT_3D('',#19879,#16117,#16118);
#14050=AXIS2_PLACEMENT_3D('',#19882,#16119,#16120);
#14051=AXIS2_PLACEMENT_3D('',#19883,#16121,#16122);
#14052=AXIS2_PLACEMENT_3D('',#19886,#16123,#16124);
#14053=AXIS2_PLACEMENT_3D('',#19887,#16125,#16126);
#14054=AXIS2_PLACEMENT_3D('',#19890,#16127,#16128);
#14055=AXIS2_PLACEMENT_3D('',#19891,#16129,#16130);
#14056=AXIS2_PLACEMENT_3D('',#19894,#16131,#16132);
#14057=AXIS2_PLACEMENT_3D('',#19895,#16133,#16134);
#14058=AXIS2_PLACEMENT_3D('',#19896,#16135,#16136);
#14059=AXIS2_PLACEMENT_3D('',#19922,#16137,#16138);
#14060=AXIS2_PLACEMENT_3D('',#19946,#16139,#16140);
#14061=AXIS2_PLACEMENT_3D('',#19947,#16141,#16142);
#14062=AXIS2_PLACEMENT_3D('',#19949,#16143,#16144);
#14063=AXIS2_PLACEMENT_3D('',#19974,#16145,#16146);
#14064=AXIS2_PLACEMENT_3D('',#19999,#16147,#16148);
#14065=AXIS2_PLACEMENT_3D('',#20015,#16150,#16151);
#14066=AXIS2_PLACEMENT_3D('',#20030,#16152,#16153);
#14067=AXIS2_PLACEMENT_3D('',#20055,#16154,#16155);
#14068=AXIS2_PLACEMENT_3D('',#20080,#16156,#16157);
#14069=AXIS2_PLACEMENT_3D('',#20105,#16158,#16159);
#14070=AXIS2_PLACEMENT_3D('',#20129,#16160,#16161);
#14071=AXIS2_PLACEMENT_3D('',#20130,#16162,#16163);
#14072=AXIS2_PLACEMENT_3D('',#20132,#16164,#16165);
#14073=AXIS2_PLACEMENT_3D('',#20133,#16166,#16167);
#14074=AXIS2_PLACEMENT_3D('',#20134,#16168,#16169);
#14075=AXIS2_PLACEMENT_3D('',#20158,#16170,#16171);
#14076=AXIS2_PLACEMENT_3D('',#20159,#16172,#16173);
#14077=AXIS2_PLACEMENT_3D('',#20161,#16174,#16175);
#14078=AXIS2_PLACEMENT_3D('',#20162,#16176,#16177);
#14079=AXIS2_PLACEMENT_3D('',#20163,#16178,#16179);
#14080=AXIS2_PLACEMENT_3D('',#20187,#16180,#16181);
#14081=AXIS2_PLACEMENT_3D('',#20188,#16182,#16183);
#14082=AXIS2_PLACEMENT_3D('',#20190,#16184,#16185);
#14083=AXIS2_PLACEMENT_3D('',#20191,#16186,#16187);
#14084=AXIS2_PLACEMENT_3D('',#20192,#16188,#16189);
#14085=AXIS2_PLACEMENT_3D('',#20207,#16190,#16191);
#14086=AXIS2_PLACEMENT_3D('',#20220,#16192,#16193);
#14087=AXIS2_PLACEMENT_3D('',#20222,#16194,#16195);
#14088=AXIS2_PLACEMENT_3D('',#20223,#16196,#16197);
#14089=AXIS2_PLACEMENT_3D('',#20224,#16198,#16199);
#14090=AXIS2_PLACEMENT_3D('',#20248,#16200,#16201);
#14091=AXIS2_PLACEMENT_3D('',#20249,#16202,#16203);
#14092=AXIS2_PLACEMENT_3D('',#20251,#16204,#16205);
#14093=AXIS2_PLACEMENT_3D('',#20252,#16206,#16207);
#14094=AXIS2_PLACEMENT_3D('',#20253,#16208,#16209);
#14095=AXIS2_PLACEMENT_3D('',#20277,#16210,#16211);
#14096=AXIS2_PLACEMENT_3D('',#20278,#16212,#16213);
#14097=AXIS2_PLACEMENT_3D('',#20280,#16214,#16215);
#14098=AXIS2_PLACEMENT_3D('',#20281,#16216,#16217);
#14099=AXIS2_PLACEMENT_3D('',#20282,#16218,#16219);
#14100=AXIS2_PLACEMENT_3D('',#20306,#16220,#16221);
#14101=AXIS2_PLACEMENT_3D('',#20307,#16222,#16223);
#14102=AXIS2_PLACEMENT_3D('',#20309,#16224,#16225);
#14103=AXIS2_PLACEMENT_3D('',#20312,#16227,#16228);
#14104=AXIS2_PLACEMENT_3D('',#20336,#16229,#16230);
#14105=AXIS2_PLACEMENT_3D('',#20337,#16231,#16232);
#14106=AXIS2_PLACEMENT_3D('',#20338,#16233,#16234);
#14107=AXIS2_PLACEMENT_3D('',#20339,#16235,#16236);
#14108=AXIS2_PLACEMENT_3D('',#20340,#16237,#16238);
#14109=AXIS2_PLACEMENT_3D('',#20341,#16239,#16240);
#14110=AXIS2_PLACEMENT_3D('',#20342,#16241,#16242);
#14111=AXIS2_PLACEMENT_3D('',#20343,#16243,#16244);
#14112=AXIS2_PLACEMENT_3D('',#20344,#16245,#16246);
#14113=AXIS2_PLACEMENT_3D('',#20346,#16247,#16248);
#14114=AXIS2_PLACEMENT_3D('',#20348,#16249,#16250);
#14115=AXIS2_PLACEMENT_3D('',#20349,#16251,#16252);
#14116=AXIS2_PLACEMENT_3D('',#20351,#16253,#16254);
#14117=AXIS2_PLACEMENT_3D('',#20353,#16256,#16257);
#14118=AXIS2_PLACEMENT_3D('',#20355,#16258,#16259);
#14119=AXIS2_PLACEMENT_3D('',#20356,#16260,#16261);
#14120=AXIS2_PLACEMENT_3D('',#20358,#16263,#16264);
#14121=AXIS2_PLACEMENT_3D('',#20360,#16265,#16266);
#14122=AXIS2_PLACEMENT_3D('',#20362,#16267,#16268);
#14123=AXIS2_PLACEMENT_3D('',#20363,#16269,#16270);
#14124=AXIS2_PLACEMENT_3D('',#20365,#16271,#16272);
#14125=AXIS2_PLACEMENT_3D('',#20367,#16274,#16275);
#14126=AXIS2_PLACEMENT_3D('',#20369,#16276,#16277);
#14127=AXIS2_PLACEMENT_3D('',#20370,#16278,#16279);
#14128=AXIS2_PLACEMENT_3D('',#20372,#16281,#16282);
#14129=AXIS2_PLACEMENT_3D('',#20373,#16283,#16284);
#14130=AXIS2_PLACEMENT_3D('',#20374,#16285,#16286);
#14131=AXIS2_PLACEMENT_3D('',#20375,#16287,#16288);
#14132=AXIS2_PLACEMENT_3D('',#20376,#16289,#16290);
#14133=AXIS2_PLACEMENT_3D('',#20377,#16291,#16292);
#14134=AXIS2_PLACEMENT_3D('',#20378,#16293,#16294);
#14135=AXIS2_PLACEMENT_3D('',#20387,#16299,#16300);
#14136=AXIS2_PLACEMENT_3D('',#20393,#16304,#16305);
#14137=AXIS2_PLACEMENT_3D('',#20399,#16309,#16310);
#14138=AXIS2_PLACEMENT_3D('',#20405,#16314,#16315);
#14139=AXIS2_PLACEMENT_3D('',#20411,#16319,#16320);
#14140=AXIS2_PLACEMENT_3D('',#20417,#16324,#16325);
#14141=AXIS2_PLACEMENT_3D('',#20423,#16329,#16330);
#14142=AXIS2_PLACEMENT_3D('',#20429,#16334,#16335);
#14143=AXIS2_PLACEMENT_3D('',#20435,#16339,#16340);
#14144=AXIS2_PLACEMENT_3D('',#20444,#16345,#16346);
#14145=AXIS2_PLACEMENT_3D('',#20450,#16350,#16351);
#14146=AXIS2_PLACEMENT_3D('',#20456,#16355,#16356);
#14147=AXIS2_PLACEMENT_3D('',#20462,#16360,#16361);
#14148=AXIS2_PLACEMENT_3D('',#20468,#16365,#16366);
#14149=AXIS2_PLACEMENT_3D('',#20474,#16370,#16371);
#14150=AXIS2_PLACEMENT_3D('',#20480,#16375,#16376);
#14151=AXIS2_PLACEMENT_3D('',#20486,#16380,#16381);
#14152=AXIS2_PLACEMENT_3D('',#20492,#16385,#16386);
#14153=AXIS2_PLACEMENT_3D('',#20501,#16391,#16392);
#14154=AXIS2_PLACEMENT_3D('',#20507,#16396,#16397);
#14155=AXIS2_PLACEMENT_3D('',#20513,#16401,#16402);
#14156=AXIS2_PLACEMENT_3D('',#20519,#16406,#16407);
#14157=AXIS2_PLACEMENT_3D('',#20525,#16411,#16412);
#14158=AXIS2_PLACEMENT_3D('',#20531,#16416,#16417);
#14159=AXIS2_PLACEMENT_3D('',#20537,#16421,#16422);
#14160=AXIS2_PLACEMENT_3D('',#20543,#16426,#16427);
#14161=AXIS2_PLACEMENT_3D('',#20549,#16431,#16432);
#14162=AXIS2_PLACEMENT_3D('',#20558,#16437,#16438);
#14163=AXIS2_PLACEMENT_3D('',#20564,#16442,#16443);
#14164=AXIS2_PLACEMENT_3D('',#20570,#16447,#16448);
#14165=AXIS2_PLACEMENT_3D('',#20576,#16452,#16453);
#14166=AXIS2_PLACEMENT_3D('',#20582,#16457,#16458);
#14167=AXIS2_PLACEMENT_3D('',#20588,#16462,#16463);
#14168=AXIS2_PLACEMENT_3D('',#20594,#16467,#16468);
#14169=AXIS2_PLACEMENT_3D('',#20600,#16472,#16473);
#14170=AXIS2_PLACEMENT_3D('',#20606,#16477,#16478);
#14171=AXIS2_PLACEMENT_3D('',#20608,#16479,#16480);
#14172=AXIS2_PLACEMENT_3D('',#20611,#16482,#16483);
#14173=AXIS2_PLACEMENT_3D('',#20612,#16484,#16485);
#14174=AXIS2_PLACEMENT_3D('',#20618,#16489,#16490);
#14175=AXIS2_PLACEMENT_3D('',#20624,#16494,#16495);
#14176=AXIS2_PLACEMENT_3D('',#20627,#16498,#16499);
#14177=AXIS2_PLACEMENT_3D('',#20633,#16503,#16504);
#14178=AXIS2_PLACEMENT_3D('',#20636,#16507,#16508);
#14179=AXIS2_PLACEMENT_3D('',#20642,#16512,#16513);
#14180=AXIS2_PLACEMENT_3D('',#20645,#16516,#16517);
#14181=AXIS2_PLACEMENT_3D('',#20648,#16520,#16521);
#14182=AXIS2_PLACEMENT_3D('',#20649,#16522,#16523);
#14183=AXIS2_PLACEMENT_3D('',#20650,#16524,#16525);
#14184=AXIS2_PLACEMENT_3D('',#20651,#16526,#16527);
#14185=AXIS2_PLACEMENT_3D('',#20662,#16532,#16533);
#14186=AXIS2_PLACEMENT_3D('',#20664,#16535,#16536);
#14187=AXIS2_PLACEMENT_3D('',#20666,#16537,#16538);
#14188=AXIS2_PLACEMENT_3D('',#20669,#16540,#16541);
#14189=AXIS2_PLACEMENT_3D('',#20671,#16542,#16543);
#14190=AXIS2_PLACEMENT_3D('',#20673,#16544,#16545);
#14191=AXIS2_PLACEMENT_3D('',#20674,#16546,#16547);
#14192=AXIS2_PLACEMENT_3D('',#20675,#16548,#16549);
#14193=AXIS2_PLACEMENT_3D('',#20679,#16552,#16553);
#14194=AXIS2_PLACEMENT_3D('',#20683,#16556,#16557);
#14195=AXIS2_PLACEMENT_3D('',#20689,#16561,#16562);
#14196=AXIS2_PLACEMENT_3D('',#20695,#16566,#16567);
#14197=AXIS2_PLACEMENT_3D('',#20699,#16570,#16571);
#14198=AXIS2_PLACEMENT_3D('',#20703,#16574,#16575);
#14199=AXIS2_PLACEMENT_3D('',#20705,#16577,#16578);
#14200=AXIS2_PLACEMENT_3D('',#20706,#16579,#16580);
#14201=AXIS2_PLACEMENT_3D('',#20707,#16581,#16582);
#14202=AXIS2_PLACEMENT_3D('',#20709,#16583,#16584);
#14203=AXIS2_PLACEMENT_3D('',#20712,#16586,#16587);
#14204=AXIS2_PLACEMENT_3D('',#20713,#16588,#16589);
#14205=AXIS2_PLACEMENT_3D('',#20716,#16591,#16592);
#14206=AXIS2_PLACEMENT_3D('',#20717,#16593,#16594);
#14207=AXIS2_PLACEMENT_3D('',#20719,#16595,#16596);
#14208=AXIS2_PLACEMENT_3D('',#20720,#16597,#16598);
#14209=AXIS2_PLACEMENT_3D('',#20723,#16600,#16601);
#14210=AXIS2_PLACEMENT_3D('',#20724,#16602,#16603);
#14211=AXIS2_PLACEMENT_3D('',#20725,#16604,#16605);
#14212=AXIS2_PLACEMENT_3D('',#20726,#16606,#16607);
#14213=AXIS2_PLACEMENT_3D('',#20735,#16612,#16613);
#14214=AXIS2_PLACEMENT_3D('',#20741,#16617,#16618);
#14215=AXIS2_PLACEMENT_3D('',#20747,#16622,#16623);
#14216=AXIS2_PLACEMENT_3D('',#20753,#16627,#16628);
#14217=AXIS2_PLACEMENT_3D('',#20759,#16632,#16633);
#14218=AXIS2_PLACEMENT_3D('',#20762,#16636,#16637);
#14219=AXIS2_PLACEMENT_3D('',#20763,#16638,#16639);
#14220=AXIS2_PLACEMENT_3D('',#20764,#16640,#16641);
#14221=AXIS2_PLACEMENT_3D('',#20766,#16642,#16643);
#14222=AXIS2_PLACEMENT_3D('',#20767,#16644,#16645);
#14223=AXIS2_PLACEMENT_3D('',#20769,#16646,#16647);
#14224=AXIS2_PLACEMENT_3D('',#20770,#16648,#16649);
#14225=AXIS2_PLACEMENT_3D('',#20772,#16650,#16651);
#14226=AXIS2_PLACEMENT_3D('',#20774,#16653,#16654);
#14227=AXIS2_PLACEMENT_3D('',#20776,#16655,#16656);
#14228=AXIS2_PLACEMENT_3D('',#20778,#16658,#16659);
#14229=AXIS2_PLACEMENT_3D('',#20780,#16660,#16661);
#14230=AXIS2_PLACEMENT_3D('',#20782,#16663,#16664);
#14231=AXIS2_PLACEMENT_3D('',#20784,#16665,#16666);
#14232=AXIS2_PLACEMENT_3D('',#20785,#16667,#16668);
#14233=AXIS2_PLACEMENT_3D('',#20787,#16669,#16670);
#14234=AXIS2_PLACEMENT_3D('',#20789,#16672,#16673);
#14235=AXIS2_PLACEMENT_3D('',#20791,#16675,#16676);
#14236=AXIS2_PLACEMENT_3D('',#20792,#16677,#16678);
#14237=AXIS2_PLACEMENT_3D('',#20793,#16679,#16680);
#14238=AXIS2_PLACEMENT_3D('',#20795,#16681,#16682);
#14239=AXIS2_PLACEMENT_3D('',#20798,#16684,#16685);
#14240=AXIS2_PLACEMENT_3D('',#20799,#16686,#16687);
#14241=AXIS2_PLACEMENT_3D('',#20801,#16688,#16689);
#14242=AXIS2_PLACEMENT_3D('',#20804,#16691,#16692);
#14243=AXIS2_PLACEMENT_3D('',#20805,#16693,#16694);
#14244=AXIS2_PLACEMENT_3D('',#20807,#16695,#16696);
#14245=AXIS2_PLACEMENT_3D('',#20810,#16698,#16699);
#14246=AXIS2_PLACEMENT_3D('',#20811,#16700,#16701);
#14247=AXIS2_PLACEMENT_3D('',#20813,#16702,#16703);
#14248=AXIS2_PLACEMENT_3D('',#20816,#16705,#16706);
#14249=AXIS2_PLACEMENT_3D('',#20817,#16707,#16708);
#14250=AXIS2_PLACEMENT_3D('',#20826,#16713,#16714);
#14251=AXIS2_PLACEMENT_3D('',#20832,#16718,#16719);
#14252=AXIS2_PLACEMENT_3D('',#20838,#16723,#16724);
#14253=AXIS2_PLACEMENT_3D('',#20841,#16727,#16728);
#14254=AXIS2_PLACEMENT_3D('',#20842,#16729,#16730);
#14255=AXIS2_PLACEMENT_3D('',#20843,#16731,#16732);
#14256=AXIS2_PLACEMENT_3D('',#20844,#16733,#16734);
#14257=AXIS2_PLACEMENT_3D('',#20846,#16735,#16736);
#14258=AXIS2_PLACEMENT_3D('',#20849,#16738,#16739);
#14259=AXIS2_PLACEMENT_3D('',#20850,#16740,#16741);
#14260=AXIS2_PLACEMENT_3D('',#20852,#16742,#16743);
#14261=AXIS2_PLACEMENT_3D('',#20855,#16745,#16746);
#14262=AXIS2_PLACEMENT_3D('',#20856,#16747,#16748);
#14263=AXIS2_PLACEMENT_3D('',#20858,#16749,#16750);
#14264=AXIS2_PLACEMENT_3D('',#20861,#16752,#16753);
#14265=AXIS2_PLACEMENT_3D('',#20862,#16754,#16755);
#14266=AXIS2_PLACEMENT_3D('',#20864,#16756,#16757);
#14267=AXIS2_PLACEMENT_3D('',#20867,#16759,#16760);
#14268=AXIS2_PLACEMENT_3D('',#20868,#16761,#16762);
#14269=AXIS2_PLACEMENT_3D('',#20870,#16763,#16764);
#14270=AXIS2_PLACEMENT_3D('',#20873,#16766,#16767);
#14271=AXIS2_PLACEMENT_3D('',#20874,#16768,#16769);
#14272=AXIS2_PLACEMENT_3D('',#20876,#16770,#16771);
#14273=AXIS2_PLACEMENT_3D('',#20879,#16773,#16774);
#14274=AXIS2_PLACEMENT_3D('',#20880,#16775,#16776);
#14275=AXIS2_PLACEMENT_3D('',#20882,#16777,#16778);
#14276=AXIS2_PLACEMENT_3D('',#20885,#16780,#16781);
#14277=AXIS2_PLACEMENT_3D('',#20886,#16782,#16783);
#14278=AXIS2_PLACEMENT_3D('',#20888,#16784,#16785);
#14279=AXIS2_PLACEMENT_3D('',#20891,#16787,#16788);
#14280=AXIS2_PLACEMENT_3D('',#20892,#16789,#16790);
#14281=AXIS2_PLACEMENT_3D('',#20901,#16795,#16796);
#14282=AXIS2_PLACEMENT_3D('',#20907,#16800,#16801);
#14283=AXIS2_PLACEMENT_3D('',#20913,#16805,#16806);
#14284=AXIS2_PLACEMENT_3D('',#20916,#16809,#16810);
#14285=AXIS2_PLACEMENT_3D('',#20917,#16811,#16812);
#14286=AXIS2_PLACEMENT_3D('',#20918,#16813,#16814);
#14287=AXIS2_PLACEMENT_3D('',#20919,#16815,#16816);
#14288=AXIS2_PLACEMENT_3D('',#20921,#16817,#16818);
#14289=AXIS2_PLACEMENT_3D('',#20924,#16820,#16821);
#14290=AXIS2_PLACEMENT_3D('',#20925,#16822,#16823);
#14291=AXIS2_PLACEMENT_3D('',#20926,#16824,#16825);
#14292=AXIS2_PLACEMENT_3D('',#20928,#16826,#16827);
#14293=AXIS2_PLACEMENT_3D('',#20931,#16829,#16830);
#14294=AXIS2_PLACEMENT_3D('',#20932,#16831,#16832);
#14295=AXIS2_PLACEMENT_3D('',#20933,#16833,#16834);
#14296=AXIS2_PLACEMENT_3D('',#20935,#16835,#16836);
#14297=AXIS2_PLACEMENT_3D('',#20938,#16838,#16839);
#14298=AXIS2_PLACEMENT_3D('',#20939,#16840,#16841);
#14299=AXIS2_PLACEMENT_3D('',#20940,#16842,#16843);
#14300=AXIS2_PLACEMENT_3D('',#20942,#16844,#16845);
#14301=AXIS2_PLACEMENT_3D('',#20945,#16847,#16848);
#14302=AXIS2_PLACEMENT_3D('',#20946,#16849,#16850);
#14303=AXIS2_PLACEMENT_3D('',#20947,#16851,#16852);
#14304=AXIS2_PLACEMENT_3D('',#20949,#16853,#16854);
#14305=AXIS2_PLACEMENT_3D('',#20952,#16856,#16857);
#14306=AXIS2_PLACEMENT_3D('',#20953,#16858,#16859);
#14307=AXIS2_PLACEMENT_3D('',#20954,#16860,#16861);
#14308=AXIS2_PLACEMENT_3D('',#20956,#16862,#16863);
#14309=AXIS2_PLACEMENT_3D('',#20959,#16865,#16866);
#14310=AXIS2_PLACEMENT_3D('',#20960,#16867,#16868);
#14311=AXIS2_PLACEMENT_3D('',#20961,#16869,#16870);
#14312=AXIS2_PLACEMENT_3D('',#20963,#16871,#16872);
#14313=AXIS2_PLACEMENT_3D('',#20966,#16874,#16875);
#14314=AXIS2_PLACEMENT_3D('',#20967,#16876,#16877);
#14315=AXIS2_PLACEMENT_3D('',#20968,#16878,#16879);
#14316=AXIS2_PLACEMENT_3D('',#20970,#16880,#16881);
#14317=AXIS2_PLACEMENT_3D('',#20973,#16883,#16884);
#14318=AXIS2_PLACEMENT_3D('',#20974,#16885,#16886);
#14319=AXIS2_PLACEMENT_3D('',#20983,#16891,#16892);
#14320=AXIS2_PLACEMENT_3D('',#20989,#16896,#16897);
#14321=AXIS2_PLACEMENT_3D('',#20995,#16901,#16902);
#14322=AXIS2_PLACEMENT_3D('',#20998,#16905,#16906);
#14323=AXIS2_PLACEMENT_3D('',#20999,#16907,#16908);
#14324=AXIS2_PLACEMENT_3D('',#21000,#16909,#16910);
#14325=AXIS2_PLACEMENT_3D('',#21001,#16911,#16912);
#14326=AXIS2_PLACEMENT_3D('',#21002,#16913,#16914);
#14327=AXIS2_PLACEMENT_3D('',#21006,#16916,#16917);
#14328=AXIS2_PLACEMENT_3D('',#21007,#16918,#16919);
#14329=AXIS2_PLACEMENT_3D('',#21011,#16921,#16922);
#14330=AXIS2_PLACEMENT_3D('',#21014,#16924,#16925);
#14331=AXIS2_PLACEMENT_3D('',#21016,#16926,#16927);
#14332=AXIS2_PLACEMENT_3D('',#21018,#16929,#16930);
#14333=AXIS2_PLACEMENT_3D('',#21022,#16932,#16933);
#14334=AXIS2_PLACEMENT_3D('',#21023,#16934,#16935);
#14335=AXIS2_PLACEMENT_3D('',#21027,#16937,#16938);
#14336=AXIS2_PLACEMENT_3D('',#21030,#16940,#16941);
#14337=AXIS2_PLACEMENT_3D('',#21032,#16942,#16943);
#14338=AXIS2_PLACEMENT_3D('',#21034,#16945,#16946);
#14339=AXIS2_PLACEMENT_3D('',#21038,#16948,#16949);
#14340=AXIS2_PLACEMENT_3D('',#21039,#16950,#16951);
#14341=AXIS2_PLACEMENT_3D('',#21043,#16953,#16954);
#14342=AXIS2_PLACEMENT_3D('',#21046,#16956,#16957);
#14343=AXIS2_PLACEMENT_3D('',#21048,#16958,#16959);
#14344=AXIS2_PLACEMENT_3D('',#21050,#16961,#16962);
#14345=AXIS2_PLACEMENT_3D('',#21054,#16964,#16965);
#14346=AXIS2_PLACEMENT_3D('',#21055,#16966,#16967);
#14347=AXIS2_PLACEMENT_3D('',#21059,#16969,#16970);
#14348=AXIS2_PLACEMENT_3D('',#21062,#16972,#16973);
#14349=AXIS2_PLACEMENT_3D('',#21064,#16974,#16975);
#14350=AXIS2_PLACEMENT_3D('',#21066,#16977,#16978);
#14351=AXIS2_PLACEMENT_3D('',#21077,#16985,#16986);
#14352=AXIS2_PLACEMENT_3D('',#21088,#16993,#16994);
#14353=AXIS2_PLACEMENT_3D('',#21107,#17005,#17006);
#14354=AXIS2_PLACEMENT_3D('',#21111,#17009,#17010);
#14355=AXIS2_PLACEMENT_3D('',#21115,#17013,#17014);
#14356=AXIS2_PLACEMENT_3D('',#21119,#17017,#17018);
#14357=AXIS2_PLACEMENT_3D('',#21123,#17021,#17022);
#14358=AXIS2_PLACEMENT_3D('',#21125,#17024,#17025);
#14359=AXIS2_PLACEMENT_3D('',#21129,#17028,#17029);
#14360=AXIS2_PLACEMENT_3D('',#21133,#17032,#17033);
#14361=AXIS2_PLACEMENT_3D('',#21137,#17036,#17037);
#14362=AXIS2_PLACEMENT_3D('',#21141,#17040,#17041);
#14363=AXIS2_PLACEMENT_3D('',#21143,#17043,#17044);
#14364=AXIS2_PLACEMENT_3D('',#21144,#17045,#17046);
#14365=AXIS2_PLACEMENT_3D('',#21145,#17047,#17048);
#14366=AXIS2_PLACEMENT_3D('',#21154,#17053,#17054);
#14367=AXIS2_PLACEMENT_3D('',#21160,#17058,#17059);
#14368=AXIS2_PLACEMENT_3D('',#21166,#17063,#17064);
#14369=AXIS2_PLACEMENT_3D('',#21172,#17068,#17069);
#14370=AXIS2_PLACEMENT_3D('',#21178,#17073,#17074);
#14371=AXIS2_PLACEMENT_3D('',#21184,#17078,#17079);
#14372=AXIS2_PLACEMENT_3D('',#21190,#17083,#17084);
#14373=AXIS2_PLACEMENT_3D('',#21193,#17087,#17088);
#14374=AXIS2_PLACEMENT_3D('',#21194,#17089,#17090);
#14375=AXIS2_PLACEMENT_3D('',#21195,#17091,#17092);
#14376=AXIS2_PLACEMENT_3D('',#21196,#17093,#17094);
#14377=AXIS2_PLACEMENT_3D('',#21205,#17099,#17100);
#14378=AXIS2_PLACEMENT_3D('',#21211,#17104,#17105);
#14379=AXIS2_PLACEMENT_3D('',#21217,#17109,#17110);
#14380=AXIS2_PLACEMENT_3D('',#21223,#17114,#17115);
#14381=AXIS2_PLACEMENT_3D('',#21229,#17119,#17120);
#14382=AXIS2_PLACEMENT_3D('',#21235,#17124,#17125);
#14383=AXIS2_PLACEMENT_3D('',#21241,#17129,#17130);
#14384=AXIS2_PLACEMENT_3D('',#21244,#17133,#17134);
#14385=AXIS2_PLACEMENT_3D('',#21245,#17135,#17136);
#14386=AXIS2_PLACEMENT_3D('',#21246,#17137,#17138);
#14387=AXIS2_PLACEMENT_3D('',#21247,#17139,#17140);
#14388=AXIS2_PLACEMENT_3D('',#21248,#17141,#17142);
#14389=AXIS2_PLACEMENT_3D('',#21249,#17143,#17144);
#14390=AXIS2_PLACEMENT_3D('',#21250,#17145,#17146);
#14391=AXIS2_PLACEMENT_3D('',#21252,#17147,#17148);
#14392=AXIS2_PLACEMENT_3D('',#21255,#17150,#17151);
#14393=AXIS2_PLACEMENT_3D('',#21256,#17152,#17153);
#14394=AXIS2_PLACEMENT_3D('',#21259,#17155,#17156);
#14395=AXIS2_PLACEMENT_3D('',#21260,#17157,#17158);
#14396=AXIS2_PLACEMENT_3D('',#21262,#17159,#17160);
#14397=AXIS2_PLACEMENT_3D('',#21263,#17161,#17162);
#14398=AXIS2_PLACEMENT_3D('',#21266,#17164,#17165);
#14399=AXIS2_PLACEMENT_3D('',#21267,#17166,#17167);
#14400=AXIS2_PLACEMENT_3D('',#21268,#17168,#17169);
#14401=AXIS2_PLACEMENT_3D('',#21269,#17170,#17171);
#14402=AXIS2_PLACEMENT_3D('',#21278,#17176,#17177);
#14403=AXIS2_PLACEMENT_3D('',#21284,#17181,#17182);
#14404=AXIS2_PLACEMENT_3D('',#21290,#17186,#17187);
#14405=AXIS2_PLACEMENT_3D('',#21296,#17191,#17192);
#14406=AXIS2_PLACEMENT_3D('',#21302,#17196,#17197);
#14407=AXIS2_PLACEMENT_3D('',#21305,#17200,#17201);
#14408=AXIS2_PLACEMENT_3D('',#21306,#17202,#17203);
#14409=AXIS2_PLACEMENT_3D('',#21307,#17204,#17205);
#14410=AXIS2_PLACEMENT_3D('',#21309,#17206,#17207);
#14411=AXIS2_PLACEMENT_3D('',#21311,#17208,#17209);
#14412=AXIS2_PLACEMENT_3D('',#21312,#17210,#17211);
#14413=AXIS2_PLACEMENT_3D('',#21315,#17213,#17214);
#14414=AXIS2_PLACEMENT_3D('',#21316,#17215,#17216);
#14415=AXIS2_PLACEMENT_3D('',#21317,#17217,#17218);
#14416=AXIS2_PLACEMENT_3D('',#21319,#17219,#17220);
#14417=AXIS2_PLACEMENT_3D('',#21320,#17221,#17222);
#14418=AXIS2_PLACEMENT_3D('',#21322,#17223,#17224);
#14419=AXIS2_PLACEMENT_3D('',#21324,#17226,#17227);
#14420=AXIS2_PLACEMENT_3D('',#21326,#17228,#17229);
#14421=AXIS2_PLACEMENT_3D('',#21328,#17231,#17232);
#14422=AXIS2_PLACEMENT_3D('',#21330,#17233,#17234);
#14423=AXIS2_PLACEMENT_3D('',#21332,#17236,#17237);
#14424=AXIS2_PLACEMENT_3D('',#21334,#17238,#17239);
#14425=AXIS2_PLACEMENT_3D('',#21335,#17240,#17241);
#14426=AXIS2_PLACEMENT_3D('',#21337,#17242,#17243);
#14427=AXIS2_PLACEMENT_3D('',#21339,#17245,#17246);
#14428=AXIS2_PLACEMENT_3D('',#21341,#17248,#17249);
#14429=AXIS2_PLACEMENT_3D('',#21342,#17250,#17251);
#14430=AXIS2_PLACEMENT_3D('',#21373,#17253,#17254);
#14431=AXIS2_PLACEMENT_3D('',#21414,#17255,#17256);
#14432=AXIS2_PLACEMENT_3D('',#21501,#17258,#17259);
#14433=AXIS2_PLACEMENT_3D('',#21591,#17261,#17262);
#14434=AXIS2_PLACEMENT_3D('',#21678,#17264,#17265);
#14435=AXIS2_PLACEMENT_3D('',#21768,#17267,#17268);
#14436=AXIS2_PLACEMENT_3D('',#21855,#17270,#17271);
#14437=AXIS2_PLACEMENT_3D('',#21942,#17273,#17274);
#14438=AXIS2_PLACEMENT_3D('',#22032,#17276,#17277);
#14439=AXIS2_PLACEMENT_3D('',#22037,#17279,#17280);
#14440=AXIS2_PLACEMENT_3D('',#22048,#17281,#17282);
#14441=AXIS2_PLACEMENT_3D('',#22061,#17284,#17285);
#14442=AXIS2_PLACEMENT_3D('',#22074,#17286,#17287);
#14443=AXIS2_PLACEMENT_3D('',#22111,#17289,#17290);
#14444=AXIS2_PLACEMENT_3D('',#22148,#17292,#17293);
#14445=AXIS2_PLACEMENT_3D('',#22186,#17295,#17296);
#14446=AXIS2_PLACEMENT_3D('',#22223,#17298,#17299);
#14447=AXIS2_PLACEMENT_3D('',#22260,#17301,#17302);
#14448=AXIS2_PLACEMENT_3D('',#22298,#17304,#17305);
#14449=AXIS2_PLACEMENT_3D('',#22336,#17307,#17308);
#14450=AXIS2_PLACEMENT_3D('',#22347,#17310,#17311);
#14451=AXIS2_PLACEMENT_3D('',#22358,#17312,#17313);
#14452=AXIS2_PLACEMENT_3D('',#23501,#17314,#17315);
#14453=AXIS2_PLACEMENT_3D('',#23505,#17317,#17318);
#14454=AXIS2_PLACEMENT_3D('',#23506,#17319,#17320);
#14455=AXIS2_PLACEMENT_3D('',#23508,#17321,#17322);
#14456=AXIS2_PLACEMENT_3D('',#23510,#17323,#17324);
#14457=AXIS2_PLACEMENT_3D('',#23512,#17325,#17326);
#14458=AXIS2_PLACEMENT_3D('',#23513,#17327,#17328);
#14459=AXIS2_PLACEMENT_3D('',#23515,#17329,#17330);
#14460=AXIS2_PLACEMENT_3D('',#23517,#17332,#17333);
#14461=AXIS2_PLACEMENT_3D('',#23519,#17334,#17335);
#14462=AXIS2_PLACEMENT_3D('',#23521,#17337,#17338);
#14463=AXIS2_PLACEMENT_3D('',#23523,#17339,#17340);
#14464=AXIS2_PLACEMENT_3D('',#23525,#17342,#17343);
#14465=AXIS2_PLACEMENT_3D('',#23531,#17347,#17348);
#14466=AXIS2_PLACEMENT_3D('',#23532,#17349,#17350);
#14467=AXIS2_PLACEMENT_3D('',#23534,#17351,#17352);
#14468=AXIS2_PLACEMENT_3D('',#23535,#17353,#17354);
#14469=AXIS2_PLACEMENT_3D('',#23536,#17355,#17356);
#14470=AXIS2_PLACEMENT_3D('',#23537,#17357,#17358);
#14471=AXIS2_PLACEMENT_3D('',#23540,#17360,#17361);
#14472=AXIS2_PLACEMENT_3D('',#23541,#17362,#17363);
#14473=AXIS2_PLACEMENT_3D('',#23542,#17364,#17365);
#14474=AXIS2_PLACEMENT_3D('',#23543,#17366,#17367);
#14475=AXIS2_PLACEMENT_3D('',#23545,#17368,#17369);
#14476=AXIS2_PLACEMENT_3D('',#23546,#17370,#17371);
#14477=AXIS2_PLACEMENT_3D('',#23548,#17372,#17373);
#14478=AXIS2_PLACEMENT_3D('',#23550,#17375,#17376);
#14479=AXIS2_PLACEMENT_3D('',#23552,#17377,#17378);
#14480=AXIS2_PLACEMENT_3D('',#23554,#17380,#17381);
#14481=AXIS2_PLACEMENT_3D('',#23556,#17382,#17383);
#14482=AXIS2_PLACEMENT_3D('',#23558,#17385,#17386);
#14483=AXIS2_PLACEMENT_3D('',#23560,#17387,#17388);
#14484=AXIS2_PLACEMENT_3D('',#23561,#17389,#17390);
#14485=AXIS2_PLACEMENT_3D('',#23563,#17391,#17392);
#14486=AXIS2_PLACEMENT_3D('',#23565,#17394,#17395);
#14487=AXIS2_PLACEMENT_3D('',#23567,#17396,#17397);
#14488=AXIS2_PLACEMENT_3D('',#23569,#17399,#17400);
#14489=AXIS2_PLACEMENT_3D('',#23571,#17401,#17402);
#14490=AXIS2_PLACEMENT_3D('',#23573,#17404,#17405);
#14491=AXIS2_PLACEMENT_3D('',#23574,#17406,#17407);
#14492=AXIS2_PLACEMENT_3D('',#23583,#17412,#17413);
#14493=AXIS2_PLACEMENT_3D('',#23589,#17417,#17418);
#14494=AXIS2_PLACEMENT_3D('',#23595,#17422,#17423);
#14495=AXIS2_PLACEMENT_3D('',#23601,#17427,#17428);
#14496=AXIS2_PLACEMENT_3D('',#23607,#17432,#17433);
#14497=AXIS2_PLACEMENT_3D('',#23610,#17436,#17437);
#14498=AXIS2_PLACEMENT_3D('',#23611,#17438,#17439);
#14499=AXIS2_PLACEMENT_3D('',#23612,#17440,#17441);
#14500=AXIS2_PLACEMENT_3D('',#23613,#17442,#17443);
#14501=AXIS2_PLACEMENT_3D('',#23615,#17444,#17445);
#14502=AXIS2_PLACEMENT_3D('',#23616,#17446,#17447);
#14503=AXIS2_PLACEMENT_3D('',#23618,#17448,#17449);
#14504=AXIS2_PLACEMENT_3D('',#23620,#17451,#17452);
#14505=AXIS2_PLACEMENT_3D('',#23622,#17453,#17454);
#14506=AXIS2_PLACEMENT_3D('',#23624,#17456,#17457);
#14507=AXIS2_PLACEMENT_3D('',#23626,#17458,#17459);
#14508=AXIS2_PLACEMENT_3D('',#23628,#17461,#17462);
#14509=AXIS2_PLACEMENT_3D('',#23630,#17463,#17464);
#14510=AXIS2_PLACEMENT_3D('',#23631,#17465,#17466);
#14511=AXIS2_PLACEMENT_3D('',#23633,#17467,#17468);
#14512=AXIS2_PLACEMENT_3D('',#23635,#17470,#17471);
#14513=AXIS2_PLACEMENT_3D('',#23637,#17472,#17473);
#14514=AXIS2_PLACEMENT_3D('',#23639,#17475,#17476);
#14515=AXIS2_PLACEMENT_3D('',#23641,#17477,#17478);
#14516=AXIS2_PLACEMENT_3D('',#23643,#17480,#17481);
#14517=AXIS2_PLACEMENT_3D('',#23644,#17482,#17483);
#14518=AXIS2_PLACEMENT_3D('',#23653,#17488,#17489);
#14519=AXIS2_PLACEMENT_3D('',#23659,#17493,#17494);
#14520=AXIS2_PLACEMENT_3D('',#23665,#17498,#17499);
#14521=AXIS2_PLACEMENT_3D('',#23671,#17503,#17504);
#14522=AXIS2_PLACEMENT_3D('',#23677,#17508,#17509);
#14523=AXIS2_PLACEMENT_3D('',#23680,#17512,#17513);
#14524=AXIS2_PLACEMENT_3D('',#23681,#17514,#17515);
#14525=AXIS2_PLACEMENT_3D('',#23682,#17516,#17517);
#14526=AXIS2_PLACEMENT_3D('',#23683,#17518,#17519);
#14527=AXIS2_PLACEMENT_3D('',#23684,#17520,#17521);
#14528=AXIS2_PLACEMENT_3D('',#23685,#17522,#17523);
#14529=AXIS2_PLACEMENT_3D('',#23686,#17524,#17525);
#14530=AXIS2_PLACEMENT_3D('',#23687,#17526,#17527);
#14531=AXIS2_PLACEMENT_3D('',#23688,#17528,#17529);
#14532=AXIS2_PLACEMENT_3D('',#23689,#17530,#17531);
#14533=AXIS2_PLACEMENT_3D('',#23690,#17532,#17533);
#14534=AXIS2_PLACEMENT_3D('',#23691,#17534,#17535);
#14535=AXIS2_PLACEMENT_3D('',#23692,#17536,#17537);
#14536=AXIS2_PLACEMENT_3D('',#23693,#17538,#17539);
#14537=AXIS2_PLACEMENT_3D('',#23694,#17540,#17541);
#14538=AXIS2_PLACEMENT_3D('',#23695,#17542,#17543);
#14539=AXIS2_PLACEMENT_3D('',#23696,#17544,#17545);
#14540=AXIS2_PLACEMENT_3D('',#23697,#17546,#17547);
#14541=AXIS2_PLACEMENT_3D('',#23698,#17548,#17549);
#14542=AXIS2_PLACEMENT_3D('',#23699,#17550,#17551);
#14543=AXIS2_PLACEMENT_3D('',#23700,#17552,#17553);
#14544=AXIS2_PLACEMENT_3D('',#23701,#17554,#17555);
#14545=AXIS2_PLACEMENT_3D('',#23702,#17556,#17557);
#14546=AXIS2_PLACEMENT_3D('',#23703,#17558,#17559);
#14547=AXIS2_PLACEMENT_3D('',#23704,#17560,#17561);
#14548=AXIS2_PLACEMENT_3D('',#23729,#17563,#17564);
#14549=AXIS2_PLACEMENT_3D('',#23734,#17565,#17566);
#14550=AXIS2_PLACEMENT_3D('',#23821,#17568,#17569);
#14551=AXIS2_PLACEMENT_3D('',#23911,#17571,#17572);
#14552=AXIS2_PLACEMENT_3D('',#23998,#17574,#17575);
#14553=AXIS2_PLACEMENT_3D('',#24085,#17577,#17578);
#14554=AXIS2_PLACEMENT_3D('',#24172,#17580,#17581);
#14555=AXIS2_PLACEMENT_3D('',#24259,#17583,#17584);
#14556=AXIS2_PLACEMENT_3D('',#24346,#17586,#17587);
#14557=AXIS2_PLACEMENT_3D('',#24418,#17589,#17590);
#14558=AXIS2_PLACEMENT_3D('',#24469,#17592,#17593);
#14559=AXIS2_PLACEMENT_3D('',#24517,#17595,#17596);
#14560=AXIS2_PLACEMENT_3D('',#24565,#17598,#17599);
#14561=AXIS2_PLACEMENT_3D('',#24616,#17601,#17602);
#14562=AXIS2_PLACEMENT_3D('',#24667,#17604,#17605);
#14563=AXIS2_PLACEMENT_3D('',#24715,#17607,#17608);
#14564=AXIS2_PLACEMENT_3D('',#24766,#17610,#17611);
#14565=AXIS2_PLACEMENT_3D('',#24817,#17613,#17614);
#14566=AXIS2_PLACEMENT_3D('',#24865,#17616,#17617);
#14567=AXIS2_PLACEMENT_3D('',#24913,#17619,#17620);
#14568=AXIS2_PLACEMENT_3D('',#24964,#17622,#17623);
#14569=AXIS2_PLACEMENT_3D('',#25015,#17625,#17626);
#14570=AXIS2_PLACEMENT_3D('',#25063,#17628,#17629);
#14571=AXIS2_PLACEMENT_3D('',#25114,#17631,#17632);
#14572=AXIS2_PLACEMENT_3D('',#25165,#17634,#17635);
#14573=AXIS2_PLACEMENT_3D('',#25213,#17637,#17638);
#14574=AXIS2_PLACEMENT_3D('',#25261,#17640,#17641);
#14575=AXIS2_PLACEMENT_3D('',#25312,#17643,#17644);
#14576=AXIS2_PLACEMENT_3D('',#25363,#17646,#17647);
#14577=AXIS2_PLACEMENT_3D('',#25411,#17649,#17650);
#14578=AXIS2_PLACEMENT_3D('',#25462,#17652,#17653);
#14579=AXIS2_PLACEMENT_3D('',#25513,#17655,#17656);
#14580=AXIS2_PLACEMENT_3D('',#25561,#17658,#17659);
#14581=AXIS2_PLACEMENT_3D('',#25609,#17661,#17662);
#14582=AXIS2_PLACEMENT_3D('',#25660,#17664,#17665);
#14583=AXIS2_PLACEMENT_3D('',#25711,#17667,#17668);
#14584=AXIS2_PLACEMENT_3D('',#25759,#17670,#17671);
#14585=AXIS2_PLACEMENT_3D('',#25810,#17673,#17674);
#14586=AXIS2_PLACEMENT_3D('',#25861,#17676,#17677);
#14587=AXIS2_PLACEMENT_3D('',#25909,#17679,#17680);
#14588=AXIS2_PLACEMENT_3D('',#25957,#17682,#17683);
#14589=AXIS2_PLACEMENT_3D('',#26008,#17685,#17686);
#14590=AXIS2_PLACEMENT_3D('',#26059,#17688,#17689);
#14591=AXIS2_PLACEMENT_3D('',#26107,#17691,#17692);
#14592=AXIS2_PLACEMENT_3D('',#26158,#17694,#17695);
#14593=AXIS2_PLACEMENT_3D('',#26209,#17697,#17698);
#14594=AXIS2_PLACEMENT_3D('',#26257,#17700,#17701);
#14595=AXIS2_PLACEMENT_3D('',#26305,#17703,#17704);
#14596=AXIS2_PLACEMENT_3D('',#26356,#17706,#17707);
#14597=AXIS2_PLACEMENT_3D('',#26407,#17709,#17710);
#14598=AXIS2_PLACEMENT_3D('',#26455,#17712,#17713);
#14599=AXIS2_PLACEMENT_3D('',#26506,#17715,#17716);
#14600=AXIS2_PLACEMENT_3D('',#26557,#17718,#17719);
#14601=AXIS2_PLACEMENT_3D('',#26605,#17721,#17722);
#14602=AXIS2_PLACEMENT_3D('',#26653,#17724,#17725);
#14603=AXIS2_PLACEMENT_3D('',#26704,#17727,#17728);
#14604=AXIS2_PLACEMENT_3D('',#26770,#17730,#17731);
#14605=AXIS2_PLACEMENT_3D('',#26860,#17733,#17734);
#14606=AXIS2_PLACEMENT_3D('',#26947,#17736,#17737);
#14607=AXIS2_PLACEMENT_3D('',#27034,#17739,#17740);
#14608=AXIS2_PLACEMENT_3D('',#27121,#17742,#17743);
#14609=AXIS2_PLACEMENT_3D('',#27208,#17745,#17746);
#14610=AXIS2_PLACEMENT_3D('',#27295,#17748,#17749);
#14611=AXIS2_PLACEMENT_3D('',#27385,#17751,#17752);
#14612=AXIS2_PLACEMENT_3D('',#27394,#17754,#17755);
#14613=AXIS2_PLACEMENT_3D('',#27395,#17756,#17757);
#14614=AXIS2_PLACEMENT_3D('',#27417,#17759,#17760);
#14615=AXIS2_PLACEMENT_3D('',#27431,#17761,#17762);
#14616=AXIS2_PLACEMENT_3D('',#27469,#17764,#17765);
#14617=AXIS2_PLACEMENT_3D('',#27505,#17767,#17768);
#14618=AXIS2_PLACEMENT_3D('',#27543,#17770,#17771);
#14619=AXIS2_PLACEMENT_3D('',#27579,#17773,#17774);
#14620=AXIS2_PLACEMENT_3D('',#27617,#17776,#17777);
#14621=AXIS2_PLACEMENT_3D('',#27654,#17779,#17780);
#14622=AXIS2_PLACEMENT_3D('',#27689,#17782,#17783);
#14623=AXIS2_PLACEMENT_3D('',#27716,#17785,#17786);
#14624=AXIS2_PLACEMENT_3D('',#27740,#17788,#17789);
#14625=AXIS2_PLACEMENT_3D('',#27764,#17791,#17792);
#14626=AXIS2_PLACEMENT_3D('',#27788,#17794,#17795);
#14627=AXIS2_PLACEMENT_3D('',#27814,#17797,#17798);
#14628=AXIS2_PLACEMENT_3D('',#27838,#17800,#17801);
#14629=AXIS2_PLACEMENT_3D('',#27862,#17803,#17804);
#14630=AXIS2_PLACEMENT_3D('',#27888,#17806,#17807);
#14631=AXIS2_PLACEMENT_3D('',#27912,#17809,#17810);
#14632=AXIS2_PLACEMENT_3D('',#27936,#17812,#17813);
#14633=AXIS2_PLACEMENT_3D('',#27960,#17815,#17816);
#14634=AXIS2_PLACEMENT_3D('',#27986,#17818,#17819);
#14635=AXIS2_PLACEMENT_3D('',#28010,#17821,#17822);
#14636=AXIS2_PLACEMENT_3D('',#28034,#17824,#17825);
#14637=AXIS2_PLACEMENT_3D('',#28060,#17827,#17828);
#14638=AXIS2_PLACEMENT_3D('',#28084,#17830,#17831);
#14639=AXIS2_PLACEMENT_3D('',#28108,#17833,#17834);
#14640=AXIS2_PLACEMENT_3D('',#28132,#17836,#17837);
#14641=AXIS2_PLACEMENT_3D('',#28158,#17839,#17840);
#14642=AXIS2_PLACEMENT_3D('',#28182,#17842,#17843);
#14643=AXIS2_PLACEMENT_3D('',#28206,#17845,#17846);
#14644=AXIS2_PLACEMENT_3D('',#28232,#17848,#17849);
#14645=AXIS2_PLACEMENT_3D('',#28256,#17851,#17852);
#14646=AXIS2_PLACEMENT_3D('',#28280,#17854,#17855);
#14647=AXIS2_PLACEMENT_3D('',#28304,#17857,#17858);
#14648=AXIS2_PLACEMENT_3D('',#28330,#17860,#17861);
#14649=AXIS2_PLACEMENT_3D('',#28354,#17863,#17864);
#14650=AXIS2_PLACEMENT_3D('',#28378,#17866,#17867);
#14651=AXIS2_PLACEMENT_3D('',#28404,#17869,#17870);
#14652=AXIS2_PLACEMENT_3D('',#28428,#17872,#17873);
#14653=AXIS2_PLACEMENT_3D('',#28452,#17875,#17876);
#14654=AXIS2_PLACEMENT_3D('',#28476,#17878,#17879);
#14655=AXIS2_PLACEMENT_3D('',#28502,#17881,#17882);
#14656=AXIS2_PLACEMENT_3D('',#28526,#17884,#17885);
#14657=AXIS2_PLACEMENT_3D('',#28550,#17887,#17888);
#14658=AXIS2_PLACEMENT_3D('',#28576,#17890,#17891);
#14659=AXIS2_PLACEMENT_3D('',#28600,#17893,#17894);
#14660=AXIS2_PLACEMENT_3D('',#28624,#17896,#17897);
#14661=AXIS2_PLACEMENT_3D('',#28648,#17899,#17900);
#14662=AXIS2_PLACEMENT_3D('',#28674,#17902,#17903);
#14663=AXIS2_PLACEMENT_3D('',#28698,#17905,#17906);
#14664=AXIS2_PLACEMENT_3D('',#28722,#17908,#17909);
#14665=AXIS2_PLACEMENT_3D('',#28748,#17911,#17912);
#14666=AXIS2_PLACEMENT_3D('',#28772,#17914,#17915);
#14667=AXIS2_PLACEMENT_3D('',#28796,#17917,#17918);
#14668=AXIS2_PLACEMENT_3D('',#28821,#17920,#17921);
#14669=AXIS2_PLACEMENT_3D('',#28848,#17923,#17924);
#14670=AXIS2_PLACEMENT_3D('',#28885,#17926,#17927);
#14671=AXIS2_PLACEMENT_3D('',#28921,#17929,#17930);
#14672=AXIS2_PLACEMENT_3D('',#28959,#17932,#17933);
#14673=AXIS2_PLACEMENT_3D('',#28995,#17935,#17936);
#14674=AXIS2_PLACEMENT_3D('',#29033,#17938,#17939);
#14675=AXIS2_PLACEMENT_3D('',#29070,#17941,#17942);
#14676=AXIS2_PLACEMENT_3D('',#29107,#17944,#17945);
#14677=AXIS2_PLACEMENT_3D('',#29109,#17946,#17947);
#14678=AXIS2_PLACEMENT_3D('',#29186,#17948,#17949);
#14679=AXIS2_PLACEMENT_3D('',#29187,#17950,#17951);
#14680=AXIS2_PLACEMENT_3D('',#29190,#17953,#17954);
#14681=AXIS2_PLACEMENT_3D('',#29191,#17955,#17956);
#14682=AXIS2_PLACEMENT_3D('',#31265,#17957,#17958);
#14683=AXIS2_PLACEMENT_3D('',#33320,#17959,#17960);
#14684=AXIS2_PLACEMENT_3D('',#33329,#17965,#17966);
#14685=AXIS2_PLACEMENT_3D('',#33331,#17967,#17968);
#14686=AXIS2_PLACEMENT_3D('',#33335,#17971,#17972);
#14687=AXIS2_PLACEMENT_3D('',#33339,#17975,#17976);
#14688=AXIS2_PLACEMENT_3D('',#33343,#17979,#17980);
#14689=AXIS2_PLACEMENT_3D('',#33344,#17981,#17982);
#14690=AXIS2_PLACEMENT_3D('',#33345,#17983,#17984);
#14691=AXIS2_PLACEMENT_3D('',#33347,#17985,#17986);
#14692=AXIS2_PLACEMENT_3D('',#33350,#17988,#17989);
#14693=AXIS2_PLACEMENT_3D('',#33351,#17990,#17991);
#14694=AXIS2_PLACEMENT_3D('',#33352,#17992,#17993);
#14695=AXIS2_PLACEMENT_3D('',#33354,#17994,#17995);
#14696=AXIS2_PLACEMENT_3D('',#33355,#17996,#17997);
#14697=AXIS2_PLACEMENT_3D('',#33356,#17998,#17999);
#14698=AXIS2_PLACEMENT_3D('',#33358,#18000,#18001);
#14699=AXIS2_PLACEMENT_3D('',#33360,#18003,#18004);
#14700=AXIS2_PLACEMENT_3D('',#33361,#18005,#18006);
#14701=AXIS2_PLACEMENT_3D('',#33362,#18007,#18008);
#14702=AXIS2_PLACEMENT_3D('',#33363,#18009,#18010);
#14703=AXIS2_PLACEMENT_3D('',#33365,#18011,#18012);
#14704=AXIS2_PLACEMENT_3D('',#33368,#18014,#18015);
#14705=AXIS2_PLACEMENT_3D('',#33369,#18016,#18017);
#14706=AXIS2_PLACEMENT_3D('',#33371,#18018,#18019);
#14707=AXIS2_PLACEMENT_3D('',#33374,#18021,#18022);
#14708=AXIS2_PLACEMENT_3D('',#33375,#18023,#18024);
#14709=AXIS2_PLACEMENT_3D('',#33376,#18025,#18026);
#14710=AXIS2_PLACEMENT_3D('',#33377,#18027,#18028);
#14711=AXIS2_PLACEMENT_3D('',#33378,#18029,#18030);
#14712=AXIS2_PLACEMENT_3D('',#33382,#18032,#18033);
#14713=AXIS2_PLACEMENT_3D('',#33383,#18034,#18035);
#14714=AXIS2_PLACEMENT_3D('',#33395,#18036,#18037);
#14715=AXIS2_PLACEMENT_3D('',#33457,#18039,#18040);
#14716=AXIS2_PLACEMENT_3D('',#33459,#18042,#18043);
#14717=AXIS2_PLACEMENT_3D('',#33461,#18044,#18045);
#14718=AXIS2_PLACEMENT_3D('',#33464,#18047,#18048);
#14719=AXIS2_PLACEMENT_3D('',#33465,#18049,#18050);
#14720=AXIS2_PLACEMENT_3D('',#33467,#18051,#18052);
#14721=AXIS2_PLACEMENT_3D('',#33470,#18054,#18055);
#14722=AXIS2_PLACEMENT_3D('',#33471,#18056,#18057);
#14723=AXIS2_PLACEMENT_3D('',#33472,#18058,#18059);
#14724=AXIS2_PLACEMENT_3D('',#33473,#18060,#18061);
#14725=AXIS2_PLACEMENT_3D('',#33474,#18062,#18063);
#14726=AXIS2_PLACEMENT_3D('',#33476,#18064,#18065);
#14727=AXIS2_PLACEMENT_3D('',#33479,#18067,#18068);
#14728=AXIS2_PLACEMENT_3D('',#33480,#18069,#18070);
#14729=AXIS2_PLACEMENT_3D('',#33484,#18072,#18073);
#14730=AXIS2_PLACEMENT_3D('',#33485,#18074,#18075);
#14731=AXIS2_PLACEMENT_3D('',#33495,#18076,#18077);
#14732=AXIS2_PLACEMENT_3D('',#33551,#18079,#18080);
#14733=AXIS2_PLACEMENT_3D('',#33553,#18082,#18083);
#14734=AXIS2_PLACEMENT_3D('',#33566,#18090,#18091);
#14735=AXIS2_PLACEMENT_3D('',#33572,#18095,#18096);
#14736=AXIS2_PLACEMENT_3D('',#33582,#18102,#18103);
#14737=AXIS2_PLACEMENT_3D('',#33584,#18104,#18105);
#14738=AXIS2_PLACEMENT_3D('',#33585,#18106,#18107);
#14739=AXIS2_PLACEMENT_3D('',#33586,#18108,#18109);
#14740=AXIS2_PLACEMENT_3D('',#33588,#18110,#18111);
#14741=AXIS2_PLACEMENT_3D('',#33589,#18112,#18113);
#14742=AXIS2_PLACEMENT_3D('',#33590,#18114,#18115);
#14743=AXIS2_PLACEMENT_3D('',#33592,#18117,#18118);
#14744=AXIS2_PLACEMENT_3D('',#33593,#18119,#18120);
#14745=AXIS2_PLACEMENT_3D('',#33594,#18121,#18122);
#14746=AXIS2_PLACEMENT_3D('',#33595,#18123,#18124);
#14747=AXIS2_PLACEMENT_3D('',#33596,#18125,#18126);
#14748=AXIS2_PLACEMENT_3D('',#33597,#18127,#18128);
#14749=AXIS2_PLACEMENT_3D('',#33598,#18129,#18130);
#14750=AXIS2_PLACEMENT_3D('',#33600,#18131,#18132);
#14751=AXIS2_PLACEMENT_3D('',#33603,#18134,#18135);
#14752=AXIS2_PLACEMENT_3D('',#33604,#18136,#18137);
#14753=AXIS2_PLACEMENT_3D('',#33606,#18138,#18139);
#14754=AXIS2_PLACEMENT_3D('',#33609,#18141,#18142);
#14755=AXIS2_PLACEMENT_3D('',#33610,#18143,#18144);
#14756=AXIS2_PLACEMENT_3D('',#33611,#18145,#18146);
#14757=AXIS2_PLACEMENT_3D('',#33612,#18147,#18148);
#14758=AXIS2_PLACEMENT_3D('',#33613,#18149,#18150);
#14759=AXIS2_PLACEMENT_3D('',#33615,#18151,#18152);
#14760=AXIS2_PLACEMENT_3D('',#33618,#18154,#18155);
#14761=AXIS2_PLACEMENT_3D('',#33619,#18156,#18157);
#14762=AXIS2_PLACEMENT_3D('',#33621,#18158,#18159);
#14763=AXIS2_PLACEMENT_3D('',#33624,#18161,#18162);
#14764=AXIS2_PLACEMENT_3D('',#33625,#18163,#18164);
#14765=AXIS2_PLACEMENT_3D('',#33626,#18165,#18166);
#14766=AXIS2_PLACEMENT_3D('',#33627,#18167,#18168);
#14767=AXIS2_PLACEMENT_3D('',#33628,#18169,#18170);
#14768=AXIS2_PLACEMENT_3D('',#33645,#18179,#18180);
#14769=AXIS2_PLACEMENT_3D('',#33651,#18184,#18185);
#14770=AXIS2_PLACEMENT_3D('',#33655,#18188,#18189);
#14771=AXIS2_PLACEMENT_3D('',#33659,#18192,#18193);
#14772=AXIS2_PLACEMENT_3D('',#33663,#18196,#18197);
#14773=AXIS2_PLACEMENT_3D('',#33671,#18202,#18203);
#14774=AXIS2_PLACEMENT_3D('',#33673,#18205,#18206);
#14775=AXIS2_PLACEMENT_3D('',#33675,#18208,#18209);
#14776=AXIS2_PLACEMENT_3D('',#33677,#18211,#18212);
#14777=AXIS2_PLACEMENT_3D('',#33678,#18213,#18214);
#14778=AXIS2_PLACEMENT_3D('',#33679,#18215,#18216);
#14779=AXIS2_PLACEMENT_3D('',#33688,#18221,#18222);
#14780=AXIS2_PLACEMENT_3D('',#33694,#18226,#18227);
#14781=AXIS2_PLACEMENT_3D('',#33700,#18231,#18232);
#14782=AXIS2_PLACEMENT_3D('',#33706,#18236,#18237);
#14783=AXIS2_PLACEMENT_3D('',#33712,#18241,#18242);
#14784=AXIS2_PLACEMENT_3D('',#33715,#18245,#18246);
#14785=AXIS2_PLACEMENT_3D('',#33716,#18247,#18248);
#14786=AXIS2_PLACEMENT_3D('',#33718,#18249,#18250);
#14787=AXIS2_PLACEMENT_3D('',#33719,#18251,#18252);
#14788=AXIS2_PLACEMENT_3D('',#33721,#18253,#18254);
#14789=AXIS2_PLACEMENT_3D('',#33723,#18256,#18257);
#14790=AXIS2_PLACEMENT_3D('',#33725,#18258,#18259);
#14791=AXIS2_PLACEMENT_3D('',#33727,#18261,#18262);
#14792=AXIS2_PLACEMENT_3D('',#33729,#18263,#18264);
#14793=AXIS2_PLACEMENT_3D('',#33731,#18266,#18267);
#14794=AXIS2_PLACEMENT_3D('',#33732,#18268,#18269);
#14795=AXIS2_PLACEMENT_3D('',#33733,#18270,#18271);
#14796=AXIS2_PLACEMENT_3D('',#33735,#18272,#18273);
#14797=AXIS2_PLACEMENT_3D('',#33738,#18275,#18276);
#14798=AXIS2_PLACEMENT_3D('',#33739,#18277,#18278);
#14799=AXIS2_PLACEMENT_3D('',#33741,#18279,#18280);
#14800=AXIS2_PLACEMENT_3D('',#33744,#18282,#18283);
#14801=AXIS2_PLACEMENT_3D('',#33745,#18284,#18285);
#14802=AXIS2_PLACEMENT_3D('',#33746,#18286,#18287);
#14803=AXIS2_PLACEMENT_3D('',#33747,#18288,#18289);
#14804=AXIS2_PLACEMENT_3D('',#33748,#18290,#18291);
#14805=AXIS2_PLACEMENT_3D('',#33750,#18292,#18293);
#14806=AXIS2_PLACEMENT_3D('',#33751,#18294,#18295);
#14807=AXIS2_PLACEMENT_3D('',#33753,#18296,#18297);
#14808=AXIS2_PLACEMENT_3D('',#33755,#18299,#18300);
#14809=AXIS2_PLACEMENT_3D('',#33757,#18301,#18302);
#14810=AXIS2_PLACEMENT_3D('',#33759,#18304,#18305);
#14811=AXIS2_PLACEMENT_3D('',#33761,#18306,#18307);
#14812=AXIS2_PLACEMENT_3D('',#33763,#18309,#18310);
#14813=AXIS2_PLACEMENT_3D('',#33765,#18311,#18312);
#14814=AXIS2_PLACEMENT_3D('',#33766,#18313,#18314);
#14815=AXIS2_PLACEMENT_3D('',#33768,#18315,#18316);
#14816=AXIS2_PLACEMENT_3D('',#33770,#18318,#18319);
#14817=AXIS2_PLACEMENT_3D('',#33772,#18320,#18321);
#14818=AXIS2_PLACEMENT_3D('',#33774,#18323,#18324);
#14819=AXIS2_PLACEMENT_3D('',#33776,#18325,#18326);
#14820=AXIS2_PLACEMENT_3D('',#33778,#18328,#18329);
#14821=AXIS2_PLACEMENT_3D('',#33779,#18330,#18331);
#14822=AXIS2_PLACEMENT_3D('',#33788,#18336,#18337);
#14823=AXIS2_PLACEMENT_3D('',#33794,#18341,#18342);
#14824=AXIS2_PLACEMENT_3D('',#33800,#18346,#18347);
#14825=AXIS2_PLACEMENT_3D('',#33806,#18351,#18352);
#14826=AXIS2_PLACEMENT_3D('',#33812,#18356,#18357);
#14827=AXIS2_PLACEMENT_3D('',#33815,#18360,#18361);
#14828=AXIS2_PLACEMENT_3D('',#33816,#18362,#18363);
#14829=AXIS2_PLACEMENT_3D('',#33817,#18364,#18365);
#14830=AXIS2_PLACEMENT_3D('',#33818,#18366,#18367);
#14831=AXIS2_PLACEMENT_3D('',#33819,#18368,#18369);
#14832=AXIS2_PLACEMENT_3D('',#33820,#18370,#18371);
#14833=AXIS2_PLACEMENT_3D('',#33821,#18372,#18373);
#14834=AXIS2_PLACEMENT_3D('',#33822,#18374,#18375);
#14835=AXIS2_PLACEMENT_3D('',#33823,#18376,#18377);
#14836=AXIS2_PLACEMENT_3D('',#33824,#18378,#18379);
#14837=AXIS2_PLACEMENT_3D('',#33825,#18380,#18381);
#14838=AXIS2_PLACEMENT_3D('',#33826,#18382,#18383);
#14839=AXIS2_PLACEMENT_3D('',#33827,#18384,#18385);
#14840=AXIS2_PLACEMENT_3D('',#33828,#18386,#18387);
#14841=AXIS2_PLACEMENT_3D('',#33829,#18388,#18389);
#14842=AXIS2_PLACEMENT_3D('',#33830,#18390,#18391);
#14843=AXIS2_PLACEMENT_3D('',#33831,#18392,#18393);
#14844=AXIS2_PLACEMENT_3D('',#33832,#18394,#18395);
#14845=AXIS2_PLACEMENT_3D('',#33833,#18396,#18397);
#14846=AXIS2_PLACEMENT_3D('',#33834,#18398,#18399);
#14847=AXIS2_PLACEMENT_3D('',#33835,#18400,#18401);
#14848=AXIS2_PLACEMENT_3D('',#33836,#18402,#18403);
#14849=AXIS2_PLACEMENT_3D('',#33837,#18404,#18405);
#14850=AXIS2_PLACEMENT_3D('',#33838,#18406,#18407);
#14851=AXIS2_PLACEMENT_3D('',#33839,#18408,#18409);
#14852=AXIS2_PLACEMENT_3D('',#33840,#18410,#18411);
#14853=AXIS2_PLACEMENT_3D('',#33841,#18412,#18413);
#14854=AXIS2_PLACEMENT_3D('',#33842,#18414,#18415);
#14855=AXIS2_PLACEMENT_3D('',#33843,#18416,#18417);
#14856=AXIS2_PLACEMENT_3D('',#33844,#18418,#18419);
#14857=AXIS2_PLACEMENT_3D('',#33845,#18420,#18421);
#14858=AXIS2_PLACEMENT_3D('',#33846,#18422,#18423);
#14859=AXIS2_PLACEMENT_3D('',#33847,#18424,#18425);
#14860=AXIS2_PLACEMENT_3D('',#33848,#18426,#18427);
#14861=AXIS2_PLACEMENT_3D('',#33849,#18428,#18429);
#14862=AXIS2_PLACEMENT_3D('',#33850,#18430,#18431);
#14863=AXIS2_PLACEMENT_3D('',#33851,#18432,#18433);
#14864=AXIS2_PLACEMENT_3D('',#33852,#18434,#18435);
#14865=AXIS2_PLACEMENT_3D('',#33853,#18436,#18437);
#14866=AXIS2_PLACEMENT_3D('',#33854,#18438,#18439);
#14867=AXIS2_PLACEMENT_3D('',#33855,#18440,#18441);
#14868=AXIS2_PLACEMENT_3D('',#33856,#18442,#18443);
#14869=AXIS2_PLACEMENT_3D('',#33857,#18444,#18445);
#14870=AXIS2_PLACEMENT_3D('',#33858,#18446,#18447);
#14871=AXIS2_PLACEMENT_3D('',#33859,#18448,#18449);
#14872=AXIS2_PLACEMENT_3D('',#33860,#18450,#18451);
#14873=AXIS2_PLACEMENT_3D('',#33861,#18452,#18453);
#14874=AXIS2_PLACEMENT_3D('',#33862,#18454,#18455);
#14875=AXIS2_PLACEMENT_3D('',#33863,#18456,#18457);
#14876=AXIS2_PLACEMENT_3D('',#33864,#18458,#18459);
#14877=AXIS2_PLACEMENT_3D('',#33865,#18460,#18461);
#14878=AXIS2_PLACEMENT_3D('',#33866,#18462,#18463);
#14879=AXIS2_PLACEMENT_3D('',#33867,#18464,#18465);
#14880=AXIS2_PLACEMENT_3D('',#33868,#18466,#18467);
#14881=AXIS2_PLACEMENT_3D('',#33869,#18468,#18469);
#14882=AXIS2_PLACEMENT_3D('',#33870,#18470,#18471);
#14883=AXIS2_PLACEMENT_3D('',#33871,#18472,#18473);
#14884=AXIS2_PLACEMENT_3D('',#33872,#18474,#18475);
#14885=AXIS2_PLACEMENT_3D('',#33873,#18476,#18477);
#14886=AXIS2_PLACEMENT_3D('',#33874,#18478,#18479);
#14887=AXIS2_PLACEMENT_3D('',#33875,#18480,#18481);
#14888=AXIS2_PLACEMENT_3D('',#33876,#18482,#18483);
#14889=AXIS2_PLACEMENT_3D('',#33877,#18484,#18485);
#14890=DIRECTION('axis',(0.,0.,1.));
#14891=DIRECTION('refdir',(1.,0.,0.));
#14892=DIRECTION('axis',(0.,0.,1.));
#14893=DIRECTION('refdir',(1.,0.,0.));
#14894=DIRECTION('axis',(0.,0.,1.));
#14895=DIRECTION('refdir',(1.,0.,0.));
#14896=DIRECTION('center_axis',(0.,0.,1.));
#14897=DIRECTION('ref_axis',(1.,0.,0.));
#14898=DIRECTION('center_axis',(0.,0.,1.));
#14899=DIRECTION('ref_axis',(1.,0.,0.));
#14900=DIRECTION('',(0.,0.,1.));
#14901=DIRECTION('center_axis',(0.,0.,-1.));
#14902=DIRECTION('ref_axis',(1.,0.,0.));
#14903=DIRECTION('center_axis',(0.,0.,1.));
#14904=DIRECTION('ref_axis',(1.,0.,0.));
#14905=DIRECTION('center_axis',(0.,0.,1.));
#14906=DIRECTION('ref_axis',(1.,0.,0.));
#14907=DIRECTION('',(0.,0.,1.));
#14908=DIRECTION('center_axis',(0.,0.,-1.));
#14909=DIRECTION('ref_axis',(1.,0.,0.));
#14910=DIRECTION('center_axis',(0.,0.,1.));
#14911=DIRECTION('ref_axis',(1.,0.,0.));
#14912=DIRECTION('center_axis',(0.,0.,1.));
#14913=DIRECTION('ref_axis',(1.,0.,0.));
#14914=DIRECTION('',(0.,0.,1.));
#14915=DIRECTION('center_axis',(0.,0.,-1.));
#14916=DIRECTION('ref_axis',(1.,0.,0.));
#14917=DIRECTION('center_axis',(0.,0.,1.));
#14918=DIRECTION('ref_axis',(1.,0.,0.));
#14919=DIRECTION('center_axis',(0.,0.,1.));
#14920=DIRECTION('ref_axis',(1.,0.,0.));
#14921=DIRECTION('',(0.,0.,1.));
#14922=DIRECTION('center_axis',(0.,0.,-1.));
#14923=DIRECTION('ref_axis',(1.,0.,0.));
#14924=DIRECTION('center_axis',(0.,0.,1.));
#14925=DIRECTION('ref_axis',(1.,0.,0.));
#14926=DIRECTION('center_axis',(0.,0.,1.));
#14927=DIRECTION('ref_axis',(1.,0.,0.));
#14928=DIRECTION('',(0.,0.,1.));
#14929=DIRECTION('center_axis',(0.,0.,-1.));
#14930=DIRECTION('ref_axis',(1.,0.,0.));
#14931=DIRECTION('center_axis',(0.,0.,1.));
#14932=DIRECTION('ref_axis',(1.,0.,0.));
#14933=DIRECTION('center_axis',(0.,0.,1.));
#14934=DIRECTION('ref_axis',(1.,0.,0.));
#14935=DIRECTION('',(0.,0.,1.));
#14936=DIRECTION('center_axis',(0.,0.,-1.));
#14937=DIRECTION('ref_axis',(1.,0.,0.));
#14938=DIRECTION('center_axis',(0.,0.,1.));
#14939=DIRECTION('ref_axis',(1.,0.,0.));
#14940=DIRECTION('center_axis',(0.,0.,1.));
#14941=DIRECTION('ref_axis',(1.,0.,0.));
#14942=DIRECTION('',(0.,0.,1.));
#14943=DIRECTION('center_axis',(0.,0.,-1.));
#14944=DIRECTION('ref_axis',(1.,0.,0.));
#14945=DIRECTION('center_axis',(0.,0.,1.));
#14946=DIRECTION('ref_axis',(1.,0.,0.));
#14947=DIRECTION('center_axis',(0.,0.,1.));
#14948=DIRECTION('ref_axis',(1.,0.,0.));
#14949=DIRECTION('',(0.,0.,1.));
#14950=DIRECTION('center_axis',(0.,0.,-1.));
#14951=DIRECTION('ref_axis',(1.,0.,0.));
#14952=DIRECTION('center_axis',(0.,0.,1.));
#14953=DIRECTION('ref_axis',(1.,0.,0.));
#14954=DIRECTION('center_axis',(0.,0.,1.));
#14955=DIRECTION('ref_axis',(1.,0.,0.));
#14956=DIRECTION('',(0.,0.,1.));
#14957=DIRECTION('center_axis',(0.,0.,-1.));
#14958=DIRECTION('ref_axis',(1.,0.,0.));
#14959=DIRECTION('center_axis',(0.,0.,1.));
#14960=DIRECTION('ref_axis',(1.,0.,0.));
#14961=DIRECTION('center_axis',(0.,0.,1.));
#14962=DIRECTION('ref_axis',(1.,0.,0.));
#14963=DIRECTION('',(0.,0.,1.));
#14964=DIRECTION('center_axis',(0.,0.,-1.));
#14965=DIRECTION('ref_axis',(1.,0.,0.));
#14966=DIRECTION('center_axis',(0.,0.,1.));
#14967=DIRECTION('ref_axis',(1.,0.,0.));
#14968=DIRECTION('center_axis',(0.,0.,1.));
#14969=DIRECTION('ref_axis',(1.,0.,0.));
#14970=DIRECTION('',(0.,0.,1.));
#14971=DIRECTION('center_axis',(0.,0.,-1.));
#14972=DIRECTION('ref_axis',(1.,0.,0.));
#14973=DIRECTION('center_axis',(0.,0.,1.));
#14974=DIRECTION('ref_axis',(1.,0.,0.));
#14975=DIRECTION('center_axis',(0.,0.,1.));
#14976=DIRECTION('ref_axis',(1.,0.,0.));
#14977=DIRECTION('',(0.,0.,1.));
#14978=DIRECTION('center_axis',(0.,0.,-1.));
#14979=DIRECTION('ref_axis',(1.,0.,0.));
#14980=DIRECTION('center_axis',(0.,0.,1.));
#14981=DIRECTION('ref_axis',(1.,0.,0.));
#14982=DIRECTION('center_axis',(0.,0.,1.));
#14983=DIRECTION('ref_axis',(1.,0.,0.));
#14984=DIRECTION('',(0.,0.,1.));
#14985=DIRECTION('center_axis',(0.,0.,-1.));
#14986=DIRECTION('ref_axis',(1.,0.,0.));
#14987=DIRECTION('center_axis',(0.,0.,1.));
#14988=DIRECTION('ref_axis',(1.,0.,0.));
#14989=DIRECTION('center_axis',(0.,0.,1.));
#14990=DIRECTION('ref_axis',(1.,0.,0.));
#14991=DIRECTION('',(0.,0.,1.));
#14992=DIRECTION('center_axis',(0.,0.,-1.));
#14993=DIRECTION('ref_axis',(1.,0.,0.));
#14994=DIRECTION('center_axis',(0.,0.,1.));
#14995=DIRECTION('ref_axis',(1.,0.,0.));
#14996=DIRECTION('center_axis',(0.,0.,1.));
#14997=DIRECTION('ref_axis',(1.,0.,0.));
#14998=DIRECTION('',(0.,0.,1.));
#14999=DIRECTION('center_axis',(0.,0.,-1.));
#15000=DIRECTION('ref_axis',(1.,0.,0.));
#15001=DIRECTION('center_axis',(0.,0.,1.));
#15002=DIRECTION('ref_axis',(1.,0.,0.));
#15003=DIRECTION('center_axis',(0.,0.,1.));
#15004=DIRECTION('ref_axis',(1.,0.,0.));
#15005=DIRECTION('',(0.,0.,1.));
#15006=DIRECTION('center_axis',(0.,0.,-1.));
#15007=DIRECTION('ref_axis',(1.,0.,0.));
#15008=DIRECTION('center_axis',(0.,1.,0.));
#15009=DIRECTION('ref_axis',(-1.,0.,0.));
#15010=DIRECTION('',(-1.,0.,0.));
#15011=DIRECTION('',(0.,0.,1.));
#15012=DIRECTION('',(-1.,0.,0.));
#15013=DIRECTION('',(0.,0.,1.));
#15014=DIRECTION('center_axis',(1.,0.,0.));
#15015=DIRECTION('ref_axis',(0.,1.,0.));
#15016=DIRECTION('',(0.,1.,0.));
#15017=DIRECTION('',(0.,1.,0.));
#15018=DIRECTION('',(0.,0.,1.));
#15019=DIRECTION('center_axis',(0.,-1.,0.));
#15020=DIRECTION('ref_axis',(1.,0.,0.));
#15021=DIRECTION('',(1.,0.,0.));
#15022=DIRECTION('',(1.,0.,0.));
#15023=DIRECTION('',(0.,0.,1.));
#15024=DIRECTION('center_axis',(-1.,0.,0.));
#15025=DIRECTION('ref_axis',(0.,-1.,0.));
#15026=DIRECTION('',(0.,-1.,0.));
#15027=DIRECTION('',(0.,-1.,0.));
#15028=DIRECTION('center_axis',(0.,0.,1.));
#15029=DIRECTION('ref_axis',(1.,0.,0.));
#15030=DIRECTION('center_axis',(0.,0.,1.));
#15031=DIRECTION('ref_axis',(1.,0.,0.));
#15032=DIRECTION('axis',(0.,0.,1.));
#15033=DIRECTION('refdir',(1.,0.,0.));
#15034=DIRECTION('center_axis',(0.,0.,1.));
#15035=DIRECTION('ref_axis',(1.,0.,0.));
#15036=DIRECTION('center_axis',(0.,0.,1.));
#15037=DIRECTION('ref_axis',(1.,0.,0.));
#15038=DIRECTION('',(0.,0.,1.));
#15039=DIRECTION('center_axis',(0.,0.,-1.));
#15040=DIRECTION('ref_axis',(1.,0.,0.));
#15041=DIRECTION('center_axis',(0.,0.,1.));
#15042=DIRECTION('ref_axis',(1.,0.,0.));
#15043=DIRECTION('center_axis',(0.,0.,1.));
#15044=DIRECTION('ref_axis',(1.,0.,0.));
#15045=DIRECTION('',(0.,0.,1.));
#15046=DIRECTION('center_axis',(0.,0.,-1.));
#15047=DIRECTION('ref_axis',(1.,0.,0.));
#15048=DIRECTION('center_axis',(0.,0.,1.));
#15049=DIRECTION('ref_axis',(1.,0.,0.));
#15050=DIRECTION('center_axis',(0.,0.,1.));
#15051=DIRECTION('ref_axis',(1.,0.,0.));
#15052=DIRECTION('',(0.,0.,1.));
#15053=DIRECTION('center_axis',(0.,0.,-1.));
#15054=DIRECTION('ref_axis',(1.,0.,0.));
#15055=DIRECTION('center_axis',(0.,0.,1.));
#15056=DIRECTION('ref_axis',(1.,0.,0.));
#15057=DIRECTION('center_axis',(0.,0.,1.));
#15058=DIRECTION('ref_axis',(1.,0.,0.));
#15059=DIRECTION('',(0.,0.,1.));
#15060=DIRECTION('center_axis',(0.,0.,-1.));
#15061=DIRECTION('ref_axis',(1.,0.,0.));
#15062=DIRECTION('center_axis',(0.,0.,1.));
#15063=DIRECTION('ref_axis',(1.,0.,0.));
#15064=DIRECTION('center_axis',(0.,0.,1.));
#15065=DIRECTION('ref_axis',(1.,0.,0.));
#15066=DIRECTION('',(0.,0.,1.));
#15067=DIRECTION('center_axis',(0.,0.,-1.));
#15068=DIRECTION('ref_axis',(1.,0.,0.));
#15069=DIRECTION('center_axis',(0.,0.,1.));
#15070=DIRECTION('ref_axis',(1.,0.,0.));
#15071=DIRECTION('center_axis',(0.,0.,1.));
#15072=DIRECTION('ref_axis',(1.,0.,0.));
#15073=DIRECTION('center_axis',(0.,0.,1.));
#15074=DIRECTION('ref_axis',(1.,0.,0.));
#15075=DIRECTION('center_axis',(0.,0.,1.));
#15076=DIRECTION('ref_axis',(1.,0.,0.));
#15077=DIRECTION('',(0.,0.,1.));
#15078=DIRECTION('center_axis',(0.,0.,-1.));
#15079=DIRECTION('ref_axis',(1.,0.,0.));
#15080=DIRECTION('center_axis',(0.,0.,1.));
#15081=DIRECTION('ref_axis',(1.,0.,0.));
#15082=DIRECTION('center_axis',(0.,0.,1.));
#15083=DIRECTION('ref_axis',(1.,0.,0.));
#15084=DIRECTION('center_axis',(0.,0.,1.));
#15085=DIRECTION('ref_axis',(1.,0.,0.));
#15086=DIRECTION('center_axis',(0.,0.,1.));
#15087=DIRECTION('ref_axis',(1.,0.,0.));
#15088=DIRECTION('',(0.,0.,1.));
#15089=DIRECTION('center_axis',(0.,0.,-1.));
#15090=DIRECTION('ref_axis',(1.,0.,0.));
#15091=DIRECTION('center_axis',(0.,0.,1.));
#15092=DIRECTION('ref_axis',(1.,0.,0.));
#15093=DIRECTION('center_axis',(0.,0.,1.));
#15094=DIRECTION('ref_axis',(1.,0.,0.));
#15095=DIRECTION('center_axis',(0.,0.,1.));
#15096=DIRECTION('ref_axis',(1.,0.,0.));
#15097=DIRECTION('center_axis',(0.,0.,1.));
#15098=DIRECTION('ref_axis',(1.,0.,0.));
#15099=DIRECTION('',(0.,0.,1.));
#15100=DIRECTION('center_axis',(0.,0.,-1.));
#15101=DIRECTION('ref_axis',(1.,0.,0.));
#15102=DIRECTION('center_axis',(0.,0.,1.));
#15103=DIRECTION('ref_axis',(1.,0.,0.));
#15104=DIRECTION('center_axis',(0.,0.,1.));
#15105=DIRECTION('ref_axis',(1.,0.,0.));
#15106=DIRECTION('center_axis',(0.,0.,1.));
#15107=DIRECTION('ref_axis',(1.,0.,0.));
#15108=DIRECTION('center_axis',(0.,0.,1.));
#15109=DIRECTION('ref_axis',(1.,0.,0.));
#15110=DIRECTION('',(0.,0.,1.));
#15111=DIRECTION('center_axis',(0.,0.,1.));
#15112=DIRECTION('ref_axis',(1.,0.,0.));
#15113=DIRECTION('center_axis',(0.,0.,1.));
#15114=DIRECTION('ref_axis',(1.,0.,0.));
#15115=DIRECTION('',(0.,0.,1.));
#15116=DIRECTION('center_axis',(0.,0.,1.));
#15117=DIRECTION('ref_axis',(1.,0.,0.));
#15118=DIRECTION('center_axis',(0.,0.,1.));
#15119=DIRECTION('ref_axis',(1.,0.,0.));
#15120=DIRECTION('',(0.,0.,1.));
#15121=DIRECTION('center_axis',(0.,0.,1.));
#15122=DIRECTION('ref_axis',(1.,0.,0.));
#15123=DIRECTION('center_axis',(0.,0.,1.));
#15124=DIRECTION('ref_axis',(1.,0.,0.));
#15125=DIRECTION('',(0.,0.,1.));
#15126=DIRECTION('center_axis',(0.,1.,0.));
#15127=DIRECTION('ref_axis',(-1.,0.,0.));
#15128=DIRECTION('',(-1.,0.,0.));
#15129=DIRECTION('',(0.,0.,1.));
#15130=DIRECTION('',(-1.,0.,0.));
#15131=DIRECTION('',(0.,0.,1.));
#15132=DIRECTION('center_axis',(1.,0.,0.));
#15133=DIRECTION('ref_axis',(0.,1.,0.));
#15134=DIRECTION('',(0.,1.,0.));
#15135=DIRECTION('',(0.,1.,0.));
#15136=DIRECTION('',(0.,0.,1.));
#15137=DIRECTION('center_axis',(0.,-1.,0.));
#15138=DIRECTION('ref_axis',(1.,0.,0.));
#15139=DIRECTION('',(1.,0.,0.));
#15140=DIRECTION('',(1.,0.,0.));
#15141=DIRECTION('',(0.,0.,1.));
#15142=DIRECTION('center_axis',(-1.,0.,0.));
#15143=DIRECTION('ref_axis',(0.,-1.,0.));
#15144=DIRECTION('',(0.,-1.,0.));
#15145=DIRECTION('',(0.,-1.,0.));
#15146=DIRECTION('center_axis',(0.,0.,1.));
#15147=DIRECTION('ref_axis',(1.,0.,0.));
#15148=DIRECTION('center_axis',(0.,0.,1.));
#15149=DIRECTION('ref_axis',(1.,0.,0.));
#15150=DIRECTION('axis',(0.,0.,1.));
#15151=DIRECTION('refdir',(1.,0.,0.));
#15152=DIRECTION('center_axis',(1.,0.,0.));
#15153=DIRECTION('ref_axis',(0.,0.,-1.));
#15154=DIRECTION('center_axis',(1.,0.,0.));
#15155=DIRECTION('ref_axis',(0.,0.,-1.));
#15156=DIRECTION('',(1.,0.,0.));
#15157=DIRECTION('center_axis',(-1.,0.,0.));
#15158=DIRECTION('ref_axis',(0.,0.,-1.));
#15159=DIRECTION('center_axis',(1.,0.,0.));
#15160=DIRECTION('ref_axis',(0.,0.,-1.));
#15161=DIRECTION('center_axis',(1.,0.,0.));
#15162=DIRECTION('ref_axis',(0.,0.,-1.));
#15163=DIRECTION('',(1.,0.,0.));
#15164=DIRECTION('center_axis',(-1.,0.,0.));
#15165=DIRECTION('ref_axis',(0.,0.,-1.));
#15166=DIRECTION('center_axis',(1.,0.,0.));
#15167=DIRECTION('ref_axis',(0.,0.,-1.));
#15168=DIRECTION('center_axis',(1.,0.,0.));
#15169=DIRECTION('ref_axis',(0.,0.,-1.));
#15170=DIRECTION('',(1.,0.,0.));
#15171=DIRECTION('center_axis',(-1.,0.,0.));
#15172=DIRECTION('ref_axis',(0.,0.,-1.));
#15173=DIRECTION('center_axis',(1.,0.,0.));
#15174=DIRECTION('ref_axis',(0.,0.,-1.));
#15175=DIRECTION('center_axis',(1.,0.,0.));
#15176=DIRECTION('ref_axis',(0.,0.,-1.));
#15177=DIRECTION('',(1.,0.,0.));
#15178=DIRECTION('center_axis',(1.,0.,0.));
#15179=DIRECTION('ref_axis',(0.,0.,-1.));
#15180=DIRECTION('center_axis',(1.,0.,0.));
#15181=DIRECTION('ref_axis',(0.,0.,-1.));
#15182=DIRECTION('center_axis',(-1.,0.,0.));
#15183=DIRECTION('ref_axis',(0.,0.,-1.));
#15184=DIRECTION('center_axis',(1.,0.,0.));
#15185=DIRECTION('ref_axis',(0.,0.,-1.));
#15186=DIRECTION('',(1.,0.,0.));
#15187=DIRECTION('center_axis',(-1.,0.,0.));
#15188=DIRECTION('ref_axis',(0.,0.,-1.));
#15189=DIRECTION('center_axis',(0.,0.,1.));
#15190=DIRECTION('ref_axis',(1.,0.,0.));
#15191=DIRECTION('center_axis',(0.,0.,1.));
#15192=DIRECTION('ref_axis',(1.,0.,0.));
#15193=DIRECTION('',(0.,0.,1.));
#15194=DIRECTION('center_axis',(0.,0.,1.));
#15195=DIRECTION('ref_axis',(1.,0.,0.));
#15196=DIRECTION('center_axis',(0.,0.,1.));
#15197=DIRECTION('ref_axis',(1.,0.,0.));
#15198=DIRECTION('center_axis',(0.,0.,1.));
#15199=DIRECTION('ref_axis',(1.,0.,0.));
#15200=DIRECTION('center_axis',(0.,0.,1.));
#15201=DIRECTION('ref_axis',(1.,0.,0.));
#15202=DIRECTION('',(0.,0.,1.));
#15203=DIRECTION('center_axis',(0.,0.,1.));
#15204=DIRECTION('ref_axis',(1.,0.,0.));
#15205=DIRECTION('center_axis',(0.,0.,1.));
#15206=DIRECTION('ref_axis',(1.,0.,0.));
#15207=DIRECTION('center_axis',(0.,1.,0.));
#15208=DIRECTION('ref_axis',(-1.,0.,0.));
#15209=DIRECTION('',(-1.,0.,0.));
#15210=DIRECTION('',(0.,0.,1.));
#15211=DIRECTION('',(-1.,0.,0.));
#15212=DIRECTION('',(0.,0.,1.));
#15213=DIRECTION('center_axis',(1.,0.,0.));
#15214=DIRECTION('ref_axis',(0.,1.,0.));
#15215=DIRECTION('',(0.,1.,0.));
#15216=DIRECTION('',(0.,1.,0.));
#15217=DIRECTION('',(0.,0.,1.));
#15218=DIRECTION('center_axis',(0.,-1.,0.));
#15219=DIRECTION('ref_axis',(1.,0.,0.));
#15220=DIRECTION('',(1.,0.,0.));
#15221=DIRECTION('',(1.,0.,0.));
#15222=DIRECTION('',(0.,0.,1.));
#15223=DIRECTION('center_axis',(-1.,0.,0.));
#15224=DIRECTION('ref_axis',(0.,-1.,0.));
#15225=DIRECTION('',(0.,-1.,0.));
#15226=DIRECTION('',(0.,-1.,0.));
#15227=DIRECTION('center_axis',(0.,0.,1.));
#15228=DIRECTION('ref_axis',(1.,0.,0.));
#15229=DIRECTION('center_axis',(0.,0.,1.));
#15230=DIRECTION('ref_axis',(1.,0.,0.));
#15231=DIRECTION('axis',(0.,0.,1.));
#15232=DIRECTION('refdir',(1.,0.,0.));
#15233=DIRECTION('center_axis',(1.,0.,0.));
#15234=DIRECTION('ref_axis',(0.,0.,-1.));
#15235=DIRECTION('center_axis',(1.,0.,0.));
#15236=DIRECTION('ref_axis',(0.,0.,-1.));
#15237=DIRECTION('',(1.,0.,0.));
#15238=DIRECTION('center_axis',(-1.,0.,0.));
#15239=DIRECTION('ref_axis',(0.,0.,-1.));
#15240=DIRECTION('center_axis',(1.,0.,0.));
#15241=DIRECTION('ref_axis',(0.,0.,-1.));
#15242=DIRECTION('center_axis',(1.,0.,0.));
#15243=DIRECTION('ref_axis',(0.,0.,-1.));
#15244=DIRECTION('',(1.,0.,0.));
#15245=DIRECTION('center_axis',(-1.,0.,0.));
#15246=DIRECTION('ref_axis',(0.,0.,-1.));
#15247=DIRECTION('center_axis',(1.,0.,0.));
#15248=DIRECTION('ref_axis',(0.,0.,-1.));
#15249=DIRECTION('center_axis',(1.,0.,0.));
#15250=DIRECTION('ref_axis',(0.,0.,-1.));
#15251=DIRECTION('',(1.,0.,0.));
#15252=DIRECTION('center_axis',(-1.,0.,0.));
#15253=DIRECTION('ref_axis',(0.,0.,-1.));
#15254=DIRECTION('center_axis',(1.,0.,0.));
#15255=DIRECTION('ref_axis',(0.,0.,-1.));
#15256=DIRECTION('center_axis',(1.,0.,0.));
#15257=DIRECTION('ref_axis',(0.,0.,-1.));
#15258=DIRECTION('',(-1.,0.,0.));
#15259=DIRECTION('center_axis',(-1.,0.,0.));
#15260=DIRECTION('ref_axis',(0.,0.,-1.));
#15261=DIRECTION('center_axis',(1.,0.,0.));
#15262=DIRECTION('ref_axis',(0.,0.,-1.));
#15263=DIRECTION('center_axis',(-1.,0.,0.));
#15264=DIRECTION('ref_axis',(0.,0.,-1.));
#15265=DIRECTION('center_axis',(1.,0.,0.));
#15266=DIRECTION('ref_axis',(0.,0.,-1.));
#15267=DIRECTION('',(-1.,0.,0.));
#15268=DIRECTION('center_axis',(-1.,0.,0.));
#15269=DIRECTION('ref_axis',(0.,0.,-1.));
#15270=DIRECTION('center_axis',(1.,0.,0.));
#15271=DIRECTION('ref_axis',(0.,0.,-1.));
#15272=DIRECTION('center_axis',(1.,0.,0.));
#15273=DIRECTION('ref_axis',(0.,0.,-1.));
#15274=DIRECTION('',(-1.,0.,0.));
#15275=DIRECTION('center_axis',(1.,0.,0.));
#15276=DIRECTION('ref_axis',(0.,0.,-1.));
#15277=DIRECTION('center_axis',(1.,0.,0.));
#15278=DIRECTION('ref_axis',(0.,0.,-1.));
#15279=DIRECTION('center_axis',(1.,0.,0.));
#15280=DIRECTION('ref_axis',(0.,0.,-1.));
#15281=DIRECTION('axis',(0.,0.,1.));
#15282=DIRECTION('refdir',(1.,0.,0.));
#15283=DIRECTION('center_axis',(1.,0.,0.));
#15284=DIRECTION('ref_axis',(0.,0.,-1.));
#15285=DIRECTION('center_axis',(1.,0.,0.));
#15286=DIRECTION('ref_axis',(0.,0.,-1.));
#15287=DIRECTION('',(1.,0.,0.));
#15288=DIRECTION('center_axis',(-1.,0.,0.));
#15289=DIRECTION('ref_axis',(0.,0.,-1.));
#15290=DIRECTION('center_axis',(1.,0.,0.));
#15291=DIRECTION('ref_axis',(0.,0.,-1.));
#15292=DIRECTION('center_axis',(1.,0.,0.));
#15293=DIRECTION('ref_axis',(0.,0.,-1.));
#15294=DIRECTION('',(1.,0.,0.));
#15295=DIRECTION('center_axis',(-1.,0.,0.));
#15296=DIRECTION('ref_axis',(0.,0.,-1.));
#15297=DIRECTION('center_axis',(1.,0.,0.));
#15298=DIRECTION('ref_axis',(0.,0.,-1.));
#15299=DIRECTION('center_axis',(1.,0.,0.));
#15300=DIRECTION('ref_axis',(0.,0.,-1.));
#15301=DIRECTION('',(1.,0.,0.));
#15302=DIRECTION('center_axis',(-1.,0.,0.));
#15303=DIRECTION('ref_axis',(0.,0.,-1.));
#15304=DIRECTION('center_axis',(1.,0.,0.));
#15305=DIRECTION('ref_axis',(0.,0.,-1.));
#15306=DIRECTION('center_axis',(1.,0.,0.));
#15307=DIRECTION('ref_axis',(0.,0.,-1.));
#15308=DIRECTION('',(1.,0.,0.));
#15309=DIRECTION('center_axis',(-1.,0.,0.));
#15310=DIRECTION('ref_axis',(0.,0.,-1.));
#15311=DIRECTION('center_axis',(1.,0.,0.));
#15312=DIRECTION('ref_axis',(0.,0.,-1.));
#15313=DIRECTION('center_axis',(1.,0.,0.));
#15314=DIRECTION('ref_axis',(0.,0.,-1.));
#15315=DIRECTION('center_axis',(1.,0.,0.));
#15316=DIRECTION('ref_axis',(0.,0.,-1.));
#15317=DIRECTION('center_axis',(1.,0.,0.));
#15318=DIRECTION('ref_axis',(0.,0.,-1.));
#15319=DIRECTION('',(1.,0.,0.));
#15320=DIRECTION('center_axis',(0.,0.,1.));
#15321=DIRECTION('ref_axis',(1.,0.,0.));
#15322=DIRECTION('center_axis',(0.,0.,1.));
#15323=DIRECTION('ref_axis',(1.,0.,0.));
#15324=DIRECTION('',(0.,0.,1.));
#15325=DIRECTION('center_axis',(0.,0.,1.));
#15326=DIRECTION('ref_axis',(1.,0.,0.));
#15327=DIRECTION('center_axis',(0.,0.,1.));
#15328=DIRECTION('ref_axis',(1.,0.,0.));
#15329=DIRECTION('center_axis',(0.,0.,1.));
#15330=DIRECTION('ref_axis',(1.,0.,0.));
#15331=DIRECTION('center_axis',(0.,0.,1.));
#15332=DIRECTION('ref_axis',(1.,0.,0.));
#15333=DIRECTION('',(0.,0.,1.));
#15334=DIRECTION('center_axis',(0.,0.,1.));
#15335=DIRECTION('ref_axis',(1.,0.,0.));
#15336=DIRECTION('center_axis',(0.,0.,1.));
#15337=DIRECTION('ref_axis',(1.,0.,0.));
#15338=DIRECTION('center_axis',(0.,1.,0.));
#15339=DIRECTION('ref_axis',(-1.,0.,0.));
#15340=DIRECTION('',(-1.,0.,0.));
#15341=DIRECTION('',(0.,0.,1.));
#15342=DIRECTION('',(-1.,0.,0.));
#15343=DIRECTION('',(0.,0.,1.));
#15344=DIRECTION('center_axis',(1.,0.,0.));
#15345=DIRECTION('ref_axis',(0.,1.,0.));
#15346=DIRECTION('',(0.,1.,0.));
#15347=DIRECTION('',(0.,1.,0.));
#15348=DIRECTION('',(0.,0.,1.));
#15349=DIRECTION('center_axis',(0.,-1.,0.));
#15350=DIRECTION('ref_axis',(1.,0.,0.));
#15351=DIRECTION('',(1.,0.,0.));
#15352=DIRECTION('',(1.,0.,0.));
#15353=DIRECTION('',(0.,0.,1.));
#15354=DIRECTION('center_axis',(-1.,0.,0.));
#15355=DIRECTION('ref_axis',(0.,-1.,0.));
#15356=DIRECTION('',(0.,-1.,0.));
#15357=DIRECTION('',(0.,-1.,0.));
#15358=DIRECTION('center_axis',(0.,0.,1.));
#15359=DIRECTION('ref_axis',(1.,0.,0.));
#15360=DIRECTION('center_axis',(0.,0.,1.));
#15361=DIRECTION('ref_axis',(1.,0.,0.));
#15362=DIRECTION('axis',(0.,0.,1.));
#15363=DIRECTION('refdir',(1.,0.,0.));
#15364=DIRECTION('center_axis',(0.,0.,1.));
#15365=DIRECTION('ref_axis',(0.,-1.,0.));
#15366=DIRECTION('',(1.,0.,0.));
#15367=DIRECTION('',(0.,-1.,0.));
#15368=DIRECTION('',(-1.,0.,0.));
#15369=DIRECTION('',(0.,1.,0.));
#15370=DIRECTION('center_axis',(1.,0.,0.));
#15371=DIRECTION('ref_axis',(0.,0.,-1.));
#15372=DIRECTION('center_axis',(1.,0.,0.));
#15373=DIRECTION('ref_axis',(0.,0.,-1.));
#15374=DIRECTION('center_axis',(1.,0.,0.));
#15375=DIRECTION('ref_axis',(0.,0.,-1.));
#15376=DIRECTION('center_axis',(1.,0.,0.));
#15377=DIRECTION('ref_axis',(0.,0.,-1.));
#15378=DIRECTION('center_axis',(1.,0.,0.));
#15379=DIRECTION('ref_axis',(0.,0.,-1.));
#15380=DIRECTION('center_axis',(1.,0.,0.));
#15381=DIRECTION('ref_axis',(0.,0.,-1.));
#15382=DIRECTION('center_axis',(1.,0.,0.));
#15383=DIRECTION('ref_axis',(0.,1.22464679914735E-16,1.));
#15384=DIRECTION('center_axis',(1.,0.,0.));
#15385=DIRECTION('ref_axis',(0.,0.,-1.));
#15386=DIRECTION('center_axis',(1.,0.,0.));
#15387=DIRECTION('ref_axis',(0.,0.,-1.));
#15388=DIRECTION('',(1.,0.,0.));
#15389=DIRECTION('center_axis',(-1.,0.,0.));
#15390=DIRECTION('ref_axis',(0.,0.,-1.));
#15391=DIRECTION('center_axis',(1.,0.,0.));
#15392=DIRECTION('ref_axis',(0.,0.,-1.));
#15393=DIRECTION('',(1.,0.,0.));
#15394=DIRECTION('center_axis',(-1.,0.,0.));
#15395=DIRECTION('ref_axis',(0.,0.,-1.));
#15396=DIRECTION('center_axis',(1.,0.,0.));
#15397=DIRECTION('ref_axis',(0.,0.,-1.));
#15398=DIRECTION('',(1.,0.,0.));
#15399=DIRECTION('center_axis',(-1.,0.,0.));
#15400=DIRECTION('ref_axis',(0.,0.,-1.));
#15401=DIRECTION('center_axis',(1.,0.,0.));
#15402=DIRECTION('ref_axis',(0.,0.,-1.));
#15403=DIRECTION('',(-1.,0.,0.));
#15404=DIRECTION('center_axis',(1.,0.,0.));
#15405=DIRECTION('ref_axis',(0.,0.,-1.));
#15406=DIRECTION('center_axis',(1.,0.,0.));
#15407=DIRECTION('ref_axis',(0.,0.,-1.));
#15408=DIRECTION('center_axis',(-1.,0.,0.));
#15409=DIRECTION('ref_axis',(0.,0.,-1.));
#15410=DIRECTION('center_axis',(1.,0.,0.));
#15411=DIRECTION('ref_axis',(0.,0.,-1.));
#15412=DIRECTION('center_axis',(-1.,0.,0.));
#15413=DIRECTION('ref_axis',(0.,0.,-1.));
#15414=DIRECTION('',(-1.,0.,0.));
#15415=DIRECTION('center_axis',(1.,0.,0.));
#15416=DIRECTION('ref_axis',(0.,0.,-1.));
#15417=DIRECTION('axis',(0.,0.,1.));
#15418=DIRECTION('refdir',(1.,0.,0.));
#15419=DIRECTION('center_axis',(0.,0.,1.));
#15420=DIRECTION('ref_axis',(1.,0.,0.));
#15421=DIRECTION('',(1.,0.,0.));
#15422=DIRECTION('center_axis',(0.,0.,1.));
#15423=DIRECTION('ref_axis',(1.,0.,0.));
#15424=DIRECTION('center_axis',(0.,0.,1.));
#15425=DIRECTION('ref_axis',(1.,0.,0.));
#15426=DIRECTION('center_axis',(0.,0.,1.));
#15427=DIRECTION('ref_axis',(1.,0.,0.));
#15428=DIRECTION('center_axis',(0.,0.,1.));
#15429=DIRECTION('ref_axis',(1.,0.,0.));
#15430=DIRECTION('',(0.,0.,-1.));
#15431=DIRECTION('center_axis',(0.,0.,1.));
#15432=DIRECTION('ref_axis',(1.,0.,0.));
#15433=DIRECTION('',(0.,0.,1.));
#15434=DIRECTION('',(0.,0.,1.));
#15435=DIRECTION('center_axis',(0.,0.,-1.));
#15436=DIRECTION('ref_axis',(1.,0.,0.));
#15437=DIRECTION('center_axis',(0.,0.,1.));
#15438=DIRECTION('ref_axis',(1.,0.,0.));
#15439=DIRECTION('',(-1.,0.,0.));
#15440=DIRECTION('center_axis',(0.,0.,1.));
#15441=DIRECTION('ref_axis',(1.,0.,0.));
#15442=DIRECTION('center_axis',(0.,0.,1.));
#15443=DIRECTION('ref_axis',(1.,0.,0.));
#15444=DIRECTION('center_axis',(0.,0.,1.));
#15445=DIRECTION('ref_axis',(1.,0.,0.));
#15446=DIRECTION('center_axis',(0.,0.,1.));
#15447=DIRECTION('ref_axis',(1.,0.,0.));
#15448=DIRECTION('',(0.,0.,-1.));
#15449=DIRECTION('center_axis',(0.,0.,1.));
#15450=DIRECTION('ref_axis',(1.,0.,0.));
#15451=DIRECTION('',(0.,0.,1.));
#15452=DIRECTION('',(0.,0.,1.));
#15453=DIRECTION('center_axis',(0.,0.,-1.));
#15454=DIRECTION('ref_axis',(1.,0.,0.));
#15455=DIRECTION('center_axis',(0.,-1.,0.));
#15456=DIRECTION('ref_axis',(0.,0.,-1.));
#15457=DIRECTION('',(1.,0.,0.));
#15458=DIRECTION('',(0.,0.,1.));
#15459=DIRECTION('',(1.,0.,0.));
#15460=DIRECTION('',(0.,0.,-1.));
#15461=DIRECTION('',(1.,0.,0.));
#15462=DIRECTION('center_axis',(0.,1.,0.));
#15463=DIRECTION('ref_axis',(0.,0.,1.));
#15464=DIRECTION('',(1.,0.,0.));
#15465=DIRECTION('',(0.,0.,1.));
#15466=DIRECTION('',(-1.,0.,0.));
#15467=DIRECTION('',(0.,0.,-1.));
#15468=DIRECTION('',(1.,0.,0.));
#15469=DIRECTION('center_axis',(0.,0.,1.));
#15470=DIRECTION('ref_axis',(1.,0.,0.));
#15471=DIRECTION('center_axis',(0.,0.,1.));
#15472=DIRECTION('ref_axis',(1.,0.,0.));
#15473=DIRECTION('',(0.,0.,1.));
#15474=DIRECTION('center_axis',(0.,0.,1.));
#15475=DIRECTION('ref_axis',(1.,0.,0.));
#15476=DIRECTION('center_axis',(0.,0.,1.));
#15477=DIRECTION('ref_axis',(1.,0.,0.));
#15478=DIRECTION('',(0.,0.,1.));
#15479=DIRECTION('center_axis',(0.,0.,1.));
#15480=DIRECTION('ref_axis',(0.,-1.,0.));
#15481=DIRECTION('',(0.,-1.,0.));
#15482=DIRECTION('',(0.,1.,0.));
#15483=DIRECTION('center_axis',(1.,0.,0.));
#15484=DIRECTION('ref_axis',(0.,1.,0.));
#15485=DIRECTION('',(0.,1.,0.));
#15486=DIRECTION('',(0.,0.,1.));
#15487=DIRECTION('',(0.,1.,0.));
#15488=DIRECTION('',(0.,0.,1.));
#15489=DIRECTION('',(0.,1.,0.));
#15490=DIRECTION('center_axis',(0.,0.,1.));
#15491=DIRECTION('ref_axis',(1.,0.,0.));
#15492=DIRECTION('',(0.,-1.,0.));
#15493=DIRECTION('',(-1.,0.,0.));
#15494=DIRECTION('center_axis',(0.,1.,0.));
#15495=DIRECTION('ref_axis',(-1.,0.,0.));
#15496=DIRECTION('',(0.,0.,1.));
#15497=DIRECTION('',(-1.,0.,0.));
#15498=DIRECTION('center_axis',(0.,-1.,0.));
#15499=DIRECTION('ref_axis',(1.,0.,0.));
#15500=DIRECTION('',(1.,0.,0.));
#15501=DIRECTION('',(1.,0.,0.));
#15502=DIRECTION('',(0.,0.,1.));
#15503=DIRECTION('center_axis',(-1.,0.,0.));
#15504=DIRECTION('ref_axis',(0.,-1.,0.));
#15505=DIRECTION('',(0.,-1.,0.));
#15506=DIRECTION('',(0.,-1.,0.));
#15507=DIRECTION('center_axis',(0.,0.,1.));
#15508=DIRECTION('ref_axis',(1.,0.,0.));
#15509=DIRECTION('center_axis',(0.,0.,1.));
#15510=DIRECTION('ref_axis',(1.,0.,0.));
#15511=DIRECTION('axis',(0.,0.,1.));
#15512=DIRECTION('refdir',(1.,0.,0.));
#15513=DIRECTION('center_axis',(0.,0.,1.));
#15514=DIRECTION('ref_axis',(1.,0.,0.));
#15515=DIRECTION('',(1.,0.,0.));
#15516=DIRECTION('center_axis',(0.,0.,1.));
#15517=DIRECTION('ref_axis',(1.,0.,0.));
#15518=DIRECTION('center_axis',(0.,0.,1.));
#15519=DIRECTION('ref_axis',(1.,0.,0.));
#15520=DIRECTION('center_axis',(0.,0.,1.));
#15521=DIRECTION('ref_axis',(1.,0.,0.));
#15522=DIRECTION('center_axis',(0.,0.,1.));
#15523=DIRECTION('ref_axis',(1.,0.,0.));
#15524=DIRECTION('',(0.,0.,-1.));
#15525=DIRECTION('center_axis',(0.,0.,1.));
#15526=DIRECTION('ref_axis',(1.,0.,0.));
#15527=DIRECTION('',(0.,0.,1.));
#15528=DIRECTION('',(0.,0.,1.));
#15529=DIRECTION('center_axis',(0.,0.,-1.));
#15530=DIRECTION('ref_axis',(1.,0.,0.));
#15531=DIRECTION('center_axis',(0.,0.,1.));
#15532=DIRECTION('ref_axis',(1.,0.,0.));
#15533=DIRECTION('',(-1.,0.,0.));
#15534=DIRECTION('center_axis',(0.,0.,1.));
#15535=DIRECTION('ref_axis',(1.,0.,0.));
#15536=DIRECTION('center_axis',(0.,0.,1.));
#15537=DIRECTION('ref_axis',(1.,0.,0.));
#15538=DIRECTION('center_axis',(0.,0.,1.));
#15539=DIRECTION('ref_axis',(1.,0.,0.));
#15540=DIRECTION('center_axis',(0.,0.,1.));
#15541=DIRECTION('ref_axis',(1.,0.,0.));
#15542=DIRECTION('',(0.,0.,-1.));
#15543=DIRECTION('center_axis',(0.,0.,1.));
#15544=DIRECTION('ref_axis',(1.,0.,0.));
#15545=DIRECTION('',(0.,0.,1.));
#15546=DIRECTION('',(0.,0.,1.));
#15547=DIRECTION('center_axis',(0.,0.,-1.));
#15548=DIRECTION('ref_axis',(1.,0.,0.));
#15549=DIRECTION('center_axis',(0.,-1.,0.));
#15550=DIRECTION('ref_axis',(0.,0.,-1.));
#15551=DIRECTION('',(1.,0.,0.));
#15552=DIRECTION('',(0.,0.,1.));
#15553=DIRECTION('',(1.,0.,0.));
#15554=DIRECTION('',(0.,0.,-1.));
#15555=DIRECTION('',(1.,0.,0.));
#15556=DIRECTION('center_axis',(0.,1.,0.));
#15557=DIRECTION('ref_axis',(0.,0.,1.));
#15558=DIRECTION('',(1.,0.,0.));
#15559=DIRECTION('',(0.,0.,1.));
#15560=DIRECTION('',(-1.,0.,0.));
#15561=DIRECTION('',(0.,0.,-1.));
#15562=DIRECTION('',(1.,0.,0.));
#15563=DIRECTION('center_axis',(0.,0.,1.));
#15564=DIRECTION('ref_axis',(1.,0.,0.));
#15565=DIRECTION('center_axis',(0.,0.,1.));
#15566=DIRECTION('ref_axis',(1.,0.,0.));
#15567=DIRECTION('',(0.,0.,1.));
#15568=DIRECTION('center_axis',(0.,0.,1.));
#15569=DIRECTION('ref_axis',(1.,0.,0.));
#15570=DIRECTION('center_axis',(0.,0.,1.));
#15571=DIRECTION('ref_axis',(1.,0.,0.));
#15572=DIRECTION('',(0.,0.,1.));
#15573=DIRECTION('center_axis',(0.,0.,1.));
#15574=DIRECTION('ref_axis',(0.,-1.,0.));
#15575=DIRECTION('',(0.,-1.,0.));
#15576=DIRECTION('',(0.,1.,0.));
#15577=DIRECTION('center_axis',(1.,0.,0.));
#15578=DIRECTION('ref_axis',(0.,1.,0.));
#15579=DIRECTION('',(0.,1.,0.));
#15580=DIRECTION('',(0.,0.,1.));
#15581=DIRECTION('',(0.,1.,0.));
#15582=DIRECTION('',(0.,0.,1.));
#15583=DIRECTION('',(0.,1.,0.));
#15584=DIRECTION('center_axis',(0.,0.,1.));
#15585=DIRECTION('ref_axis',(1.,0.,0.));
#15586=DIRECTION('',(0.,-1.,0.));
#15587=DIRECTION('',(-1.,0.,0.));
#15588=DIRECTION('center_axis',(0.,1.,0.));
#15589=DIRECTION('ref_axis',(-1.,0.,0.));
#15590=DIRECTION('',(0.,0.,1.));
#15591=DIRECTION('',(-1.,0.,0.));
#15592=DIRECTION('center_axis',(0.,-1.,0.));
#15593=DIRECTION('ref_axis',(1.,0.,0.));
#15594=DIRECTION('',(1.,0.,0.));
#15595=DIRECTION('',(1.,0.,0.));
#15596=DIRECTION('',(0.,0.,1.));
#15597=DIRECTION('center_axis',(-1.,0.,0.));
#15598=DIRECTION('ref_axis',(0.,-1.,0.));
#15599=DIRECTION('',(0.,-1.,0.));
#15600=DIRECTION('',(0.,-1.,0.));
#15601=DIRECTION('center_axis',(0.,0.,1.));
#15602=DIRECTION('ref_axis',(1.,0.,0.));
#15603=DIRECTION('center_axis',(0.,0.,1.));
#15604=DIRECTION('ref_axis',(1.,0.,0.));
#15605=DIRECTION('axis',(0.,0.,1.));
#15606=DIRECTION('refdir',(1.,0.,0.));
#15607=DIRECTION('center_axis',(0.,0.,1.));
#15608=DIRECTION('ref_axis',(1.,0.,0.));
#15609=DIRECTION('center_axis',(0.,0.,1.));
#15610=DIRECTION('ref_axis',(1.,0.,0.));
#15611=DIRECTION('',(0.,0.,1.));
#15612=DIRECTION('center_axis',(0.,0.,-1.));
#15613=DIRECTION('ref_axis',(1.,0.,0.));
#15614=DIRECTION('center_axis',(0.,0.,1.));
#15615=DIRECTION('ref_axis',(1.,0.,0.));
#15616=DIRECTION('center_axis',(0.,0.,1.));
#15617=DIRECTION('ref_axis',(1.,0.,0.));
#15618=DIRECTION('center_axis',(0.,0.,1.));
#15619=DIRECTION('ref_axis',(1.,0.,0.));
#15620=DIRECTION('center_axis',(0.,0.,1.));
#15621=DIRECTION('ref_axis',(1.,0.,0.));
#15622=DIRECTION('',(0.,0.,1.));
#15623=DIRECTION('center_axis',(0.,0.,-1.));
#15624=DIRECTION('ref_axis',(1.,0.,0.));
#15625=DIRECTION('center_axis',(0.,0.,1.));
#15626=DIRECTION('ref_axis',(1.,0.,0.));
#15627=DIRECTION('center_axis',(0.,0.,1.));
#15628=DIRECTION('ref_axis',(1.,0.,0.));
#15629=DIRECTION('center_axis',(0.,0.,1.));
#15630=DIRECTION('ref_axis',(1.,0.,0.));
#15631=DIRECTION('center_axis',(0.,0.,1.));
#15632=DIRECTION('ref_axis',(1.,0.,0.));
#15633=DIRECTION('',(0.,0.,1.));
#15634=DIRECTION('center_axis',(0.,0.,-1.));
#15635=DIRECTION('ref_axis',(1.,0.,0.));
#15636=DIRECTION('center_axis',(0.,0.,1.));
#15637=DIRECTION('ref_axis',(1.,0.,0.));
#15638=DIRECTION('center_axis',(0.,0.,1.));
#15639=DIRECTION('ref_axis',(1.,0.,0.));
#15640=DIRECTION('center_axis',(0.,0.,1.));
#15641=DIRECTION('ref_axis',(1.,0.,0.));
#15642=DIRECTION('center_axis',(0.,0.,1.));
#15643=DIRECTION('ref_axis',(1.,0.,0.));
#15644=DIRECTION('',(0.,0.,1.));
#15645=DIRECTION('center_axis',(0.,0.,-1.));
#15646=DIRECTION('ref_axis',(1.,0.,0.));
#15647=DIRECTION('center_axis',(0.,0.,1.));
#15648=DIRECTION('ref_axis',(1.,0.,0.));
#15649=DIRECTION('center_axis',(0.,0.,1.));
#15650=DIRECTION('ref_axis',(1.,0.,0.));
#15651=DIRECTION('center_axis',(0.,0.,1.));
#15652=DIRECTION('ref_axis',(1.,0.,0.));
#15653=DIRECTION('center_axis',(0.,0.,1.));
#15654=DIRECTION('ref_axis',(1.,0.,0.));
#15655=DIRECTION('',(0.,0.,1.));
#15656=DIRECTION('center_axis',(0.,0.,1.));
#15657=DIRECTION('ref_axis',(1.,0.,0.));
#15658=DIRECTION('center_axis',(0.,0.,1.));
#15659=DIRECTION('ref_axis',(1.,0.,0.));
#15660=DIRECTION('',(0.,0.,1.));
#15661=DIRECTION('center_axis',(0.,0.,1.));
#15662=DIRECTION('ref_axis',(1.,0.,0.));
#15663=DIRECTION('center_axis',(0.,0.,1.));
#15664=DIRECTION('ref_axis',(1.,0.,0.));
#15665=DIRECTION('',(0.,0.,1.));
#15666=DIRECTION('center_axis',(0.,0.,1.));
#15667=DIRECTION('ref_axis',(1.,0.,0.));
#15668=DIRECTION('center_axis',(0.,0.,1.));
#15669=DIRECTION('ref_axis',(1.,0.,0.));
#15670=DIRECTION('',(0.,0.,1.));
#15671=DIRECTION('center_axis',(0.,-0.56333682464151,0.826227342807548));
#15672=DIRECTION('ref_axis',(0.,-0.826227342807548,-0.56333682464151));
#15673=DIRECTION('',(0.,-0.826227342807548,-0.56333682464151));
#15674=DIRECTION('',(1.,0.,0.));
#15675=DIRECTION('',(0.,-0.826227342807548,-0.56333682464151));
#15676=DIRECTION('',(1.,0.,0.));
#15677=DIRECTION('center_axis',(0.,-1.,0.));
#15678=DIRECTION('ref_axis',(0.,0.,-1.));
#15679=DIRECTION('',(0.,0.,-1.));
#15680=DIRECTION('',(0.,0.,-1.));
#15681=DIRECTION('',(1.,0.,0.));
#15682=DIRECTION('center_axis',(0.,-0.56333682464151,-0.826227342807548));
#15683=DIRECTION('ref_axis',(0.,0.826227342807548,-0.56333682464151));
#15684=DIRECTION('',(0.,0.826227342807548,-0.56333682464151));
#15685=DIRECTION('',(0.,0.826227342807548,-0.56333682464151));
#15686=DIRECTION('',(1.,0.,0.));
#15687=DIRECTION('center_axis',(0.,-1.,0.));
#15688=DIRECTION('ref_axis',(0.,0.,-1.));
#15689=DIRECTION('',(0.,0.,-1.));
#15690=DIRECTION('',(0.,0.,-1.));
#15691=DIRECTION('',(1.,0.,0.));
#15692=DIRECTION('center_axis',(0.,0.,1.));
#15693=DIRECTION('ref_axis',(0.,-1.,0.));
#15694=DIRECTION('',(0.,-1.,0.));
#15695=DIRECTION('',(0.,-1.,0.));
#15696=DIRECTION('',(1.,0.,0.));
#15697=DIRECTION('center_axis',(0.,1.,0.));
#15698=DIRECTION('ref_axis',(0.,0.,1.));
#15699=DIRECTION('',(0.,0.,1.));
#15700=DIRECTION('',(0.,0.,1.));
#15701=DIRECTION('',(1.,0.,0.));
#15702=DIRECTION('center_axis',(0.,0.56333682464151,-0.826227342807548));
#15703=DIRECTION('ref_axis',(0.,0.826227342807548,0.56333682464151));
#15704=DIRECTION('',(0.,0.826227342807548,0.56333682464151));
#15705=DIRECTION('',(0.,0.826227342807548,0.56333682464151));
#15706=DIRECTION('',(1.,0.,0.));
#15707=DIRECTION('center_axis',(0.,1.,0.));
#15708=DIRECTION('ref_axis',(0.,0.,1.));
#15709=DIRECTION('',(0.,0.,1.));
#15710=DIRECTION('',(0.,0.,1.));
#15711=DIRECTION('',(1.,0.,0.));
#15712=DIRECTION('center_axis',(0.,0.56333682464151,0.826227342807548));
#15713=DIRECTION('ref_axis',(0.,-0.826227342807548,0.56333682464151));
#15714=DIRECTION('',(0.,-0.826227342807548,0.56333682464151));
#15715=DIRECTION('',(0.,-0.826227342807548,0.56333682464151));
#15716=DIRECTION('',(1.,0.,0.));
#15717=DIRECTION('center_axis',(0.,1.,0.));
#15718=DIRECTION('ref_axis',(0.,0.,1.));
#15719=DIRECTION('',(0.,0.,1.));
#15720=DIRECTION('',(0.,0.,1.));
#15721=DIRECTION('',(1.,0.,0.));
#15722=DIRECTION('center_axis',(0.,0.,-1.));
#15723=DIRECTION('ref_axis',(0.,1.,0.));
#15724=DIRECTION('',(0.,1.,0.));
#15725=DIRECTION('',(0.,1.,0.));
#15726=DIRECTION('',(1.,0.,0.));
#15727=DIRECTION('center_axis',(0.,-1.,0.));
#15728=DIRECTION('ref_axis',(0.,0.,-1.));
#15729=DIRECTION('',(0.,0.,-1.));
#15730=DIRECTION('',(0.,0.,-1.));
#15731=DIRECTION('center_axis',(1.,0.,0.));
#15732=DIRECTION('ref_axis',(0.,0.,-1.));
#15733=DIRECTION('center_axis',(1.,0.,0.));
#15734=DIRECTION('ref_axis',(0.,0.,-1.));
#15735=DIRECTION('axis',(0.,0.,1.));
#15736=DIRECTION('refdir',(1.,0.,0.));
#15737=DIRECTION('axis',(0.,0.,1.));
#15738=DIRECTION('refdir',(1.,0.,0.));
#15739=DIRECTION('center_axis',(0.,-1.,0.));
#15740=DIRECTION('ref_axis',(0.,0.,-1.));
#15741=DIRECTION('center_axis',(0.,-1.,0.));
#15742=DIRECTION('ref_axis',(1.,0.,0.));
#15743=DIRECTION('center_axis',(0.,-1.,0.));
#15744=DIRECTION('ref_axis',(1.,0.,0.));
#15745=DIRECTION('center_axis',(1.,0.,1.22464679914735E-16));
#15746=DIRECTION('ref_axis',(-1.22464679914735E-16,0.,1.));
#15747=DIRECTION('center_axis',(0.,1.,0.));
#15748=DIRECTION('ref_axis',(1.,0.,0.));
#15749=DIRECTION('center_axis',(0.,1.,0.));
#15750=DIRECTION('ref_axis',(1.,0.,0.));
#15751=DIRECTION('center_axis',(0.,-1.,0.));
#15752=DIRECTION('ref_axis',(1.,0.,0.));
#15753=DIRECTION('',(0.,1.,0.));
#15754=DIRECTION('center_axis',(0.,-1.,0.));
#15755=DIRECTION('ref_axis',(1.,0.,0.));
#15756=DIRECTION('center_axis',(0.,-1.,0.));
#15757=DIRECTION('ref_axis',(1.,0.,0.));
#15758=DIRECTION('center_axis',(0.,-1.,0.));
#15759=DIRECTION('ref_axis',(1.,0.,0.));
#15760=DIRECTION('',(0.,1.,0.));
#15761=DIRECTION('center_axis',(0.,-1.,0.));
#15762=DIRECTION('ref_axis',(1.,0.,0.));
#15763=DIRECTION('center_axis',(0.,1.,0.));
#15764=DIRECTION('ref_axis',(1.,0.,0.));
#15765=DIRECTION('',(-0.707106781186548,0.707106781186547,-8.65956056235493E-17));
#15766=DIRECTION('center_axis',(0.,-1.,0.));
#15767=DIRECTION('ref_axis',(1.,0.,0.));
#15768=DIRECTION('center_axis',(0.,1.,0.));
#15769=DIRECTION('ref_axis',(0.,0.,1.));
#15770=DIRECTION('center_axis',(0.,-1.,0.));
#15771=DIRECTION('ref_axis',(1.,0.,0.));
#15772=DIRECTION('center_axis',(0.,-1.,0.));
#15773=DIRECTION('ref_axis',(1.,0.,0.));
#15774=DIRECTION('',(0.,1.,0.));
#15775=DIRECTION('center_axis',(0.,-1.,0.));
#15776=DIRECTION('ref_axis',(0.,0.,-1.));
#15777=DIRECTION('center_axis',(0.,-1.,0.));
#15778=DIRECTION('ref_axis',(1.,0.,0.));
#15779=DIRECTION('center_axis',(0.,-1.,0.));
#15780=DIRECTION('ref_axis',(1.,0.,0.));
#15781=DIRECTION('',(0.707106781186548,0.707106781186547,8.65956056235493E-17));
#15782=DIRECTION('axis',(0.,0.,1.));
#15783=DIRECTION('refdir',(1.,0.,0.));
#15784=DIRECTION('center_axis',(0.,-1.,0.));
#15785=DIRECTION('ref_axis',(0.,0.,-1.));
#15786=DIRECTION('center_axis',(0.,-1.,0.));
#15787=DIRECTION('ref_axis',(1.,0.,0.));
#15788=DIRECTION('center_axis',(0.,-1.,0.));
#15789=DIRECTION('ref_axis',(1.,0.,0.));
#15790=DIRECTION('center_axis',(1.,0.,1.22464679914735E-16));
#15791=DIRECTION('ref_axis',(-1.22464679914735E-16,0.,1.));
#15792=DIRECTION('center_axis',(0.,1.,0.));
#15793=DIRECTION('ref_axis',(1.,0.,0.));
#15794=DIRECTION('center_axis',(0.,1.,0.));
#15795=DIRECTION('ref_axis',(1.,0.,0.));
#15796=DIRECTION('center_axis',(0.,-1.,0.));
#15797=DIRECTION('ref_axis',(1.,0.,0.));
#15798=DIRECTION('center_axis',(0.,-1.,0.));
#15799=DIRECTION('ref_axis',(1.,0.,0.));
#15800=DIRECTION('',(0.,1.,0.));
#15801=DIRECTION('center_axis',(0.,1.,0.));
#15802=DIRECTION('ref_axis',(0.,0.,1.));
#15803=DIRECTION('center_axis',(0.,-1.,0.));
#15804=DIRECTION('ref_axis',(1.,0.,0.));
#15805=DIRECTION('center_axis',(0.,-1.,0.));
#15806=DIRECTION('ref_axis',(1.,0.,0.));
#15807=DIRECTION('center_axis',(0.,-1.,0.));
#15808=DIRECTION('ref_axis',(1.,0.,0.));
#15809=DIRECTION('center_axis',(0.,-1.,0.));
#15810=DIRECTION('ref_axis',(1.,0.,0.));
#15811=DIRECTION('',(0.707106781186548,0.707106781186547,8.65956056235494E-17));
#15812=DIRECTION('center_axis',(0.,-1.,0.));
#15813=DIRECTION('ref_axis',(1.,0.,0.));
#15814=DIRECTION('center_axis',(0.,-1.,0.));
#15815=DIRECTION('ref_axis',(1.,0.,0.));
#15816=DIRECTION('',(0.,1.,0.));
#15817=DIRECTION('center_axis',(0.,1.,0.));
#15818=DIRECTION('ref_axis',(1.,0.,0.));
#15819=DIRECTION('center_axis',(0.,-1.,0.));
#15820=DIRECTION('ref_axis',(1.,0.,0.));
#15821=DIRECTION('',(-0.707106781186548,0.707106781186547,-8.65956056235494E-17));
#15822=DIRECTION('center_axis',(0.,-1.,0.));
#15823=DIRECTION('ref_axis',(0.,0.,-1.));
#15824=DIRECTION('center_axis',(0.,-1.,0.));
#15825=DIRECTION('ref_axis',(1.,0.,0.));
#15826=DIRECTION('',(0.,1.,0.));
#15827=DIRECTION('axis',(0.,0.,1.));
#15828=DIRECTION('refdir',(1.,0.,0.));
#15829=DIRECTION('center_axis',(0.,0.,1.));
#15830=DIRECTION('ref_axis',(1.,0.,0.));
#15831=DIRECTION('center_axis',(1.22464679914735E-16,-1.,0.));
#15832=DIRECTION('ref_axis',(-1.,-1.22464679914735E-16,0.));
#15833=DIRECTION('center_axis',(0.78183148246803,0.,0.623489801858733));
#15834=DIRECTION('ref_axis',(0.623489801858734,0.,-0.78183148246803));
#15835=DIRECTION('center_axis',(7.63554790147315E-17,-1.,-9.57467422477103E-17));
#15836=DIRECTION('ref_axis',(-0.623489801858734,-1.22464679914735E-16,0.78183148246803));
#15837=DIRECTION('center_axis',(0.974927912181824,0.,-0.222520933956314));
#15838=DIRECTION('ref_axis',(-0.222520933956314,0.,-0.974927912181824));
#15839=DIRECTION('center_axis',(-2.7250954951288E-17,-1.,-1.19394234705288E-16));
#15840=DIRECTION('ref_axis',(0.222520933956314,-1.22464679914735E-16,0.974927912181824));
#15841=DIRECTION('center_axis',(0.433883739117558,0.,-0.900968867902419));
#15842=DIRECTION('ref_axis',(-0.900968867902419,0.,-0.433883739117558));
#15843=DIRECTION('center_axis',(-1.10336864020811E-16,-1.,-5.31354332312403E-17));
#15844=DIRECTION('ref_axis',(0.900968867902419,-1.22464679914735E-16,0.433883739117558));
#15845=DIRECTION('center_axis',(-0.433883739117558,0.,-0.900968867902419));
#15846=DIRECTION('ref_axis',(-0.900968867902419,0.,0.433883739117558));
#15847=DIRECTION('center_axis',(-1.10336864020811E-16,-1.,5.31354332312403E-17));
#15848=DIRECTION('ref_axis',(0.900968867902419,-1.22464679914735E-16,-0.433883739117558));
#15849=DIRECTION('center_axis',(-0.974927912181824,0.,-0.222520933956314));
#15850=DIRECTION('ref_axis',(-0.222520933956315,0.,0.974927912181824));
#15851=DIRECTION('center_axis',(-2.7250954951288E-17,-1.,1.19394234705288E-16));
#15852=DIRECTION('ref_axis',(0.222520933956315,-1.22464679914735E-16,-0.974927912181824));
#15853=DIRECTION('center_axis',(-0.78183148246803,0.,0.623489801858734));
#15854=DIRECTION('ref_axis',(0.623489801858733,0.,0.78183148246803));
#15855=DIRECTION('center_axis',(7.63554790147315E-17,-1.,9.57467422477103E-17));
#15856=DIRECTION('ref_axis',(-0.623489801858733,-1.22464679914735E-16,-0.78183148246803));
#15857=DIRECTION('axis',(0.,0.,1.));
#15858=DIRECTION('refdir',(1.,0.,0.));
#15859=DIRECTION('center_axis',(0.,0.,1.));
#15860=DIRECTION('ref_axis',(1.,0.,0.));
#15861=DIRECTION('center_axis',(0.,-1.,0.));
#15862=DIRECTION('ref_axis',(0.,0.,-1.));
#15863=DIRECTION('center_axis',(0.,-1.,0.));
#15864=DIRECTION('ref_axis',(0.,0.,-1.));
#15865=DIRECTION('center_axis',(0.,1.,0.));
#15866=DIRECTION('ref_axis',(1.,0.,0.));
#15867=DIRECTION('center_axis',(0.,1.,0.));
#15868=DIRECTION('ref_axis',(1.,0.,0.));
#15869=DIRECTION('center_axis',(0.,1.,0.));
#15870=DIRECTION('ref_axis',(1.,0.,0.));
#15871=DIRECTION('center_axis',(0.,1.,0.));
#15872=DIRECTION('ref_axis',(1.,0.,0.));
#15873=DIRECTION('',(0.,-1.,0.));
#15874=DIRECTION('center_axis',(0.,-1.,0.));
#15875=DIRECTION('ref_axis',(1.,0.,0.));
#15876=DIRECTION('center_axis',(0.,1.,0.));
#15877=DIRECTION('ref_axis',(1.,0.,0.));
#15878=DIRECTION('center_axis',(0.,1.,0.));
#15879=DIRECTION('ref_axis',(1.,0.,0.));
#15880=DIRECTION('center_axis',(0.,1.,0.));
#15881=DIRECTION('ref_axis',(1.,0.,0.));
#15882=DIRECTION('center_axis',(0.,1.,0.));
#15883=DIRECTION('ref_axis',(1.,0.,0.));
#15884=DIRECTION('center_axis',(0.,1.,0.));
#15885=DIRECTION('ref_axis',(1.,0.,0.));
#15886=DIRECTION('center_axis',(0.,1.,0.));
#15887=DIRECTION('ref_axis',(1.,0.,0.));
#15888=DIRECTION('center_axis',(0.,-1.,0.));
#15889=DIRECTION('ref_axis',(1.,0.,0.));
#15890=DIRECTION('center_axis',(0.,-1.,0.));
#15891=DIRECTION('ref_axis',(0.,0.,-1.));
#15892=DIRECTION('center_axis',(8.96625347776458E-17,0.,1.));
#15893=DIRECTION('ref_axis',(1.,0.,0.));
#15894=DIRECTION('center_axis',(0.,-1.,0.));
#15895=DIRECTION('ref_axis',(0.,0.,-1.));
#15896=DIRECTION('center_axis',(0.,1.,0.));
#15897=DIRECTION('ref_axis',(1.,0.,0.));
#15898=DIRECTION('center_axis',(0.,-1.,0.));
#15899=DIRECTION('ref_axis',(1.,0.,0.));
#15900=DIRECTION('center_axis',(0.,-1.,0.));
#15901=DIRECTION('ref_axis',(0.,0.,-1.));
#15902=DIRECTION('center_axis',(0.,0.,1.));
#15903=DIRECTION('ref_axis',(1.,0.,0.));
#15904=DIRECTION('center_axis',(0.,-1.,0.));
#15905=DIRECTION('ref_axis',(0.,0.,-1.));
#15906=DIRECTION('center_axis',(0.,1.,0.));
#15907=DIRECTION('ref_axis',(1.,0.,0.));
#15908=DIRECTION('center_axis',(0.,-1.,0.));
#15909=DIRECTION('ref_axis',(1.,0.,0.));
#15910=DIRECTION('center_axis',(0.,-1.,0.));
#15911=DIRECTION('ref_axis',(1.,0.,0.));
#15912=DIRECTION('center_axis',(0.,-1.,0.));
#15913=DIRECTION('ref_axis',(0.,0.,-1.));
#15914=DIRECTION('center_axis',(0.,0.,1.));
#15915=DIRECTION('ref_axis',(1.,0.,0.));
#15916=DIRECTION('center_axis',(0.,-1.,0.));
#15917=DIRECTION('ref_axis',(0.,0.,-1.));
#15918=DIRECTION('center_axis',(0.,1.,0.));
#15919=DIRECTION('ref_axis',(1.,0.,0.));
#15920=DIRECTION('center_axis',(0.,-1.,0.));
#15921=DIRECTION('ref_axis',(1.,0.,0.));
#15922=DIRECTION('center_axis',(0.,-1.,0.));
#15923=DIRECTION('ref_axis',(0.,0.,-1.));
#15924=DIRECTION('center_axis',(8.96625347776458E-17,0.,1.));
#15925=DIRECTION('ref_axis',(1.,0.,0.));
#15926=DIRECTION('center_axis',(0.,-1.,0.));
#15927=DIRECTION('ref_axis',(0.,0.,-1.));
#15928=DIRECTION('center_axis',(0.,1.,0.));
#15929=DIRECTION('ref_axis',(1.,0.,0.));
#15930=DIRECTION('center_axis',(0.,-1.,0.));
#15931=DIRECTION('ref_axis',(1.,0.,0.));
#15932=DIRECTION('center_axis',(0.,-1.,0.));
#15933=DIRECTION('ref_axis',(0.,0.,-1.));
#15934=DIRECTION('center_axis',(0.,0.,1.));
#15935=DIRECTION('ref_axis',(1.,0.,0.));
#15936=DIRECTION('center_axis',(0.,-1.,0.));
#15937=DIRECTION('ref_axis',(0.,0.,-1.));
#15938=DIRECTION('center_axis',(0.,1.,0.));
#15939=DIRECTION('ref_axis',(1.,0.,0.));
#15940=DIRECTION('center_axis',(0.,1.,0.));
#15941=DIRECTION('ref_axis',(1.,0.,0.));
#15942=DIRECTION('',(0.,1.,0.));
#15943=DIRECTION('center_axis',(0.,-1.,0.));
#15944=DIRECTION('ref_axis',(1.,0.,0.));
#15945=DIRECTION('center_axis',(0.,-1.,0.));
#15946=DIRECTION('ref_axis',(1.,0.,0.));
#15947=DIRECTION('center_axis',(0.,1.,0.));
#15948=DIRECTION('ref_axis',(1.,0.,0.));
#15949=DIRECTION('center_axis',(0.,-1.,0.));
#15950=DIRECTION('ref_axis',(0.,0.,-1.));
#15951=DIRECTION('center_axis',(0.,0.,1.));
#15952=DIRECTION('ref_axis',(1.,0.,0.));
#15953=DIRECTION('center_axis',(0.,-1.,0.));
#15954=DIRECTION('ref_axis',(0.,0.,-1.));
#15955=DIRECTION('center_axis',(0.,-1.,0.));
#15956=DIRECTION('ref_axis',(-1.,0.,0.));
#15957=DIRECTION('center_axis',(0.,1.,0.));
#15958=DIRECTION('ref_axis',(1.,0.,0.));
#15959=DIRECTION('axis',(0.,0.,1.));
#15960=DIRECTION('refdir',(1.,0.,0.));
#15961=DIRECTION('center_axis',(0.,1.,0.));
#15962=DIRECTION('ref_axis',(0.,0.,1.));
#15963=DIRECTION('center_axis',(0.,-1.,0.));
#15964=DIRECTION('ref_axis',(1.,0.,0.));
#15965=DIRECTION('center_axis',(0.,-1.,0.));
#15966=DIRECTION('ref_axis',(1.,0.,0.));
#15967=DIRECTION('center_axis',(0.,-1.,0.));
#15968=DIRECTION('ref_axis',(1.,0.,0.));
#15969=DIRECTION('center_axis',(0.,-1.,0.));
#15970=DIRECTION('ref_axis',(1.,0.,0.));
#15971=DIRECTION('',(0.,1.,0.));
#15972=DIRECTION('center_axis',(0.,-1.,0.));
#15973=DIRECTION('ref_axis',(0.,0.,-1.));
#15974=DIRECTION('center_axis',(0.,-1.,0.));
#15975=DIRECTION('ref_axis',(1.,0.,0.));
#15976=DIRECTION('center_axis',(0.,-1.,0.));
#15977=DIRECTION('ref_axis',(1.,0.,0.));
#15978=DIRECTION('',(0.,1.,0.));
#15979=DIRECTION('center_axis',(0.,1.,0.));
#15980=DIRECTION('ref_axis',(0.,0.,1.));
#15981=DIRECTION('center_axis',(0.,-1.,0.));
#15982=DIRECTION('ref_axis',(1.,0.,0.));
#15983=DIRECTION('center_axis',(0.,-1.,0.));
#15984=DIRECTION('ref_axis',(1.,0.,0.));
#15985=DIRECTION('center_axis',(0.,-1.,0.));
#15986=DIRECTION('ref_axis',(1.,0.,0.));
#15987=DIRECTION('center_axis',(0.,-1.,0.));
#15988=DIRECTION('ref_axis',(1.,0.,0.));
#15989=DIRECTION('',(0.,1.,0.));
#15990=DIRECTION('center_axis',(0.,-1.,0.));
#15991=DIRECTION('ref_axis',(0.,0.,-1.));
#15992=DIRECTION('center_axis',(0.,-1.,0.));
#15993=DIRECTION('ref_axis',(1.,0.,0.));
#15994=DIRECTION('center_axis',(0.,-1.,0.));
#15995=DIRECTION('ref_axis',(1.,0.,0.));
#15996=DIRECTION('',(0.,1.,0.));
#15997=DIRECTION('',(0.,0.,1.));
#15998=DIRECTION('',(1.,0.,0.));
#15999=DIRECTION('',(0.,0.,1.));
#16000=DIRECTION('',(1.,0.,0.));
#16001=DIRECTION('',(0.,0.,1.));
#16002=DIRECTION('',(1.,0.,0.));
#16003=DIRECTION('',(0.,0.,1.));
#16004=DIRECTION('',(1.,0.,0.));
#16005=DIRECTION('',(0.,0.,1.));
#16006=DIRECTION('',(1.,0.,0.));
#16007=DIRECTION('axis',(0.,0.,1.));
#16008=DIRECTION('refdir',(1.,0.,0.));
#16009=DIRECTION('axis',(0.,0.,1.));
#16010=DIRECTION('refdir',(1.,0.,0.));
#16011=DIRECTION('center_axis',(0.,-1.,0.));
#16012=DIRECTION('ref_axis',(0.,0.,-1.));
#16013=DIRECTION('center_axis',(0.,-1.,0.));
#16014=DIRECTION('ref_axis',(1.,0.,0.));
#16015=DIRECTION('center_axis',(0.,-1.,0.));
#16016=DIRECTION('ref_axis',(1.,0.,0.));
#16017=DIRECTION('center_axis',(1.,0.,1.22464679914735E-16));
#16018=DIRECTION('ref_axis',(-1.22464679914735E-16,0.,1.));
#16019=DIRECTION('center_axis',(0.,1.,0.));
#16020=DIRECTION('ref_axis',(1.,0.,0.));
#16021=DIRECTION('center_axis',(0.,1.,0.));
#16022=DIRECTION('ref_axis',(1.,0.,0.));
#16023=DIRECTION('center_axis',(0.,-1.,0.));
#16024=DIRECTION('ref_axis',(1.,0.,0.));
#16025=DIRECTION('',(0.,1.,0.));
#16026=DIRECTION('center_axis',(0.,-1.,0.));
#16027=DIRECTION('ref_axis',(1.,0.,0.));
#16028=DIRECTION('center_axis',(0.,-1.,0.));
#16029=DIRECTION('ref_axis',(1.,0.,0.));
#16030=DIRECTION('center_axis',(0.,-1.,0.));
#16031=DIRECTION('ref_axis',(1.,0.,0.));
#16032=DIRECTION('',(0.,1.,0.));
#16033=DIRECTION('center_axis',(0.,-1.,0.));
#16034=DIRECTION('ref_axis',(1.,0.,0.));
#16035=DIRECTION('center_axis',(0.,1.,0.));
#16036=DIRECTION('ref_axis',(1.,0.,0.));
#16037=DIRECTION('',(-0.707106781186548,0.707106781186547,-8.65956056235494E-17));
#16038=DIRECTION('center_axis',(0.,-1.,0.));
#16039=DIRECTION('ref_axis',(1.,0.,0.));
#16040=DIRECTION('center_axis',(0.,1.,0.));
#16041=DIRECTION('ref_axis',(0.,0.,1.));
#16042=DIRECTION('center_axis',(0.,-1.,0.));
#16043=DIRECTION('ref_axis',(1.,0.,0.));
#16044=DIRECTION('center_axis',(0.,-1.,0.));
#16045=DIRECTION('ref_axis',(1.,0.,0.));
#16046=DIRECTION('',(0.,1.,0.));
#16047=DIRECTION('center_axis',(0.,-1.,0.));
#16048=DIRECTION('ref_axis',(0.,0.,-1.));
#16049=DIRECTION('center_axis',(0.,-1.,0.));
#16050=DIRECTION('ref_axis',(1.,0.,0.));
#16051=DIRECTION('center_axis',(0.,-1.,0.));
#16052=DIRECTION('ref_axis',(1.,0.,0.));
#16053=DIRECTION('',(0.707106781186548,0.707106781186547,8.65956056235494E-17));
#16054=DIRECTION('axis',(0.,0.,1.));
#16055=DIRECTION('refdir',(1.,0.,0.));
#16056=DIRECTION('center_axis',(0.,-1.,0.));
#16057=DIRECTION('ref_axis',(0.,0.,-1.));
#16058=DIRECTION('center_axis',(0.,-1.,0.));
#16059=DIRECTION('ref_axis',(1.,0.,0.));
#16060=DIRECTION('center_axis',(0.,-1.,0.));
#16061=DIRECTION('ref_axis',(1.,0.,0.));
#16062=DIRECTION('center_axis',(1.,0.,1.22464679914735E-16));
#16063=DIRECTION('ref_axis',(-1.22464679914735E-16,0.,1.));
#16064=DIRECTION('center_axis',(0.,1.,0.));
#16065=DIRECTION('ref_axis',(1.,0.,0.));
#16066=DIRECTION('center_axis',(0.,1.,0.));
#16067=DIRECTION('ref_axis',(1.,0.,0.));
#16068=DIRECTION('center_axis',(0.,-1.,0.));
#16069=DIRECTION('ref_axis',(1.,0.,0.));
#16070=DIRECTION('center_axis',(0.,-1.,0.));
#16071=DIRECTION('ref_axis',(1.,0.,0.));
#16072=DIRECTION('',(0.,1.,0.));
#16073=DIRECTION('center_axis',(0.,1.,0.));
#16074=DIRECTION('ref_axis',(0.,0.,1.));
#16075=DIRECTION('center_axis',(0.,-1.,0.));
#16076=DIRECTION('ref_axis',(1.,0.,0.));
#16077=DIRECTION('center_axis',(0.,-1.,0.));
#16078=DIRECTION('ref_axis',(1.,0.,0.));
#16079=DIRECTION('center_axis',(0.,-1.,0.));
#16080=DIRECTION('ref_axis',(1.,0.,0.));
#16081=DIRECTION('center_axis',(0.,-1.,0.));
#16082=DIRECTION('ref_axis',(1.,0.,0.));
#16083=DIRECTION('',(0.707106781186548,0.707106781186547,8.65956056235494E-17));
#16084=DIRECTION('center_axis',(0.,-1.,0.));
#16085=DIRECTION('ref_axis',(1.,0.,0.));
#16086=DIRECTION('center_axis',(0.,-1.,0.));
#16087=DIRECTION('ref_axis',(1.,0.,0.));
#16088=DIRECTION('',(0.,1.,0.));
#16089=DIRECTION('center_axis',(0.,1.,0.));
#16090=DIRECTION('ref_axis',(1.,0.,0.));
#16091=DIRECTION('center_axis',(0.,-1.,0.));
#16092=DIRECTION('ref_axis',(1.,0.,0.));
#16093=DIRECTION('',(-0.707106781186548,0.707106781186547,-8.65956056235494E-17));
#16094=DIRECTION('center_axis',(0.,-1.,0.));
#16095=DIRECTION('ref_axis',(0.,0.,-1.));
#16096=DIRECTION('center_axis',(0.,-1.,0.));
#16097=DIRECTION('ref_axis',(1.,0.,0.));
#16098=DIRECTION('',(0.,1.,0.));
#16099=DIRECTION('axis',(0.,0.,1.));
#16100=DIRECTION('refdir',(1.,0.,0.));
#16101=DIRECTION('center_axis',(0.,0.,1.));
#16102=DIRECTION('ref_axis',(1.,0.,0.));
#16103=DIRECTION('center_axis',(1.22464679914735E-16,-1.,0.));
#16104=DIRECTION('ref_axis',(-1.,-1.22464679914735E-16,0.));
#16105=DIRECTION('center_axis',(0.707106781186548,0.,0.707106781186548));
#16106=DIRECTION('ref_axis',(0.707106781186548,0.,-0.707106781186548));
#16107=DIRECTION('center_axis',(8.65956056235493E-17,-1.,-8.65956056235493E-17));
#16108=DIRECTION('ref_axis',(-0.707106781186548,-1.22464679914735E-16,0.707106781186548));
#16109=DIRECTION('center_axis',(1.,0.,0.));
#16110=DIRECTION('ref_axis',(6.12323399573677E-17,0.,-1.));
#16111=DIRECTION('center_axis',(7.49879891330929E-33,-1.,-1.22464679914735E-16));
#16112=DIRECTION('ref_axis',(-6.12323399573677E-17,-1.22464679914735E-16,
1.));
#16113=DIRECTION('center_axis',(0.707106781186548,0.,-0.707106781186548));
#16114=DIRECTION('ref_axis',(-0.707106781186548,0.,-0.707106781186548));
#16115=DIRECTION('center_axis',(-8.65956056235493E-17,-1.,-8.65956056235493E-17));
#16116=DIRECTION('ref_axis',(0.707106781186548,-1.22464679914735E-16,0.707106781186548));
#16117=DIRECTION('center_axis',(0.,0.,-1.));
#16118=DIRECTION('ref_axis',(-1.,0.,-1.22464679914735E-16));
#16119=DIRECTION('center_axis',(-1.22464679914735E-16,-1.,-1.49975978266186E-32));
#16120=DIRECTION('ref_axis',(1.,-1.22464679914735E-16,1.22464679914735E-16));
#16121=DIRECTION('center_axis',(-0.707106781186548,0.,-0.707106781186548));
#16122=DIRECTION('ref_axis',(-0.707106781186548,0.,0.707106781186548));
#16123=DIRECTION('center_axis',(-8.65956056235493E-17,-1.,8.65956056235493E-17));
#16124=DIRECTION('ref_axis',(0.707106781186548,-1.22464679914735E-16,-0.707106781186548));
#16125=DIRECTION('center_axis',(-1.,0.,0.));
#16126=DIRECTION('ref_axis',(-1.83697019872103E-16,0.,1.));
#16127=DIRECTION('center_axis',(-2.24963967399279E-32,-1.,1.22464679914735E-16));
#16128=DIRECTION('ref_axis',(1.83697019872103E-16,-1.22464679914735E-16,
-1.));
#16129=DIRECTION('center_axis',(-0.707106781186548,0.,0.707106781186548));
#16130=DIRECTION('ref_axis',(0.707106781186548,0.,0.707106781186548));
#16131=DIRECTION('center_axis',(8.65956056235493E-17,-1.,8.65956056235494E-17));
#16132=DIRECTION('ref_axis',(-0.707106781186548,-1.22464679914735E-16,-0.707106781186548));
#16133=DIRECTION('axis',(0.,0.,1.));
#16134=DIRECTION('refdir',(1.,0.,0.));
#16135=DIRECTION('center_axis',(0.,0.,1.));
#16136=DIRECTION('ref_axis',(1.,0.,0.));
#16137=DIRECTION('center_axis',(0.,-1.,0.));
#16138=DIRECTION('ref_axis',(0.,0.,-1.));
#16139=DIRECTION('center_axis',(0.,-1.,0.));
#16140=DIRECTION('ref_axis',(0.,0.,-1.));
#16141=DIRECTION('center_axis',(0.,1.,0.));
#16142=DIRECTION('ref_axis',(1.,0.,0.));
#16143=DIRECTION('center_axis',(0.,1.,0.));
#16144=DIRECTION('ref_axis',(1.,0.,0.));
#16145=DIRECTION('center_axis',(0.,1.,0.));
#16146=DIRECTION('ref_axis',(1.,0.,0.));
#16147=DIRECTION('center_axis',(0.,1.,0.));
#16148=DIRECTION('ref_axis',(1.,0.,0.));
#16149=DIRECTION('',(0.,-1.,0.));
#16150=DIRECTION('center_axis',(0.,-1.,0.));
#16151=DIRECTION('ref_axis',(1.,0.,0.));
#16152=DIRECTION('center_axis',(0.,1.,0.));
#16153=DIRECTION('ref_axis',(1.,0.,0.));
#16154=DIRECTION('center_axis',(0.,1.,0.));
#16155=DIRECTION('ref_axis',(1.,0.,0.));
#16156=DIRECTION('center_axis',(0.,1.,0.));
#16157=DIRECTION('ref_axis',(1.,0.,0.));
#16158=DIRECTION('center_axis',(0.,1.,0.));
#16159=DIRECTION('ref_axis',(1.,0.,0.));
#16160=DIRECTION('center_axis',(0.,1.,0.));
#16161=DIRECTION('ref_axis',(1.,0.,0.));
#16162=DIRECTION('center_axis',(0.,1.,0.));
#16163=DIRECTION('ref_axis',(1.,0.,0.));
#16164=DIRECTION('center_axis',(0.,-1.,0.));
#16165=DIRECTION('ref_axis',(1.,0.,0.));
#16166=DIRECTION('center_axis',(0.,-1.,0.));
#16167=DIRECTION('ref_axis',(0.,0.,-1.));
#16168=DIRECTION('center_axis',(6.12323399573677E-17,0.,1.));
#16169=DIRECTION('ref_axis',(1.,0.,0.));
#16170=DIRECTION('center_axis',(0.,-1.,0.));
#16171=DIRECTION('ref_axis',(0.,0.,-1.));
#16172=DIRECTION('center_axis',(0.,1.,0.));
#16173=DIRECTION('ref_axis',(1.,0.,0.));
#16174=DIRECTION('center_axis',(0.,-1.,0.));
#16175=DIRECTION('ref_axis',(1.,0.,0.));
#16176=DIRECTION('center_axis',(0.,-1.,0.));
#16177=DIRECTION('ref_axis',(0.,0.,-1.));
#16178=DIRECTION('center_axis',(0.,0.,1.));
#16179=DIRECTION('ref_axis',(1.,0.,0.));
#16180=DIRECTION('center_axis',(0.,-1.,0.));
#16181=DIRECTION('ref_axis',(0.,0.,-1.));
#16182=DIRECTION('center_axis',(0.,1.,0.));
#16183=DIRECTION('ref_axis',(1.,0.,0.));
#16184=DIRECTION('center_axis',(0.,-1.,0.));
#16185=DIRECTION('ref_axis',(1.,0.,0.));
#16186=DIRECTION('center_axis',(0.,-1.,0.));
#16187=DIRECTION('ref_axis',(0.,0.,-1.));
#16188=DIRECTION('center_axis',(0.,0.,1.));
#16189=DIRECTION('ref_axis',(1.,0.,0.));
#16190=DIRECTION('center_axis',(0.,-1.,0.));
#16191=DIRECTION('ref_axis',(0.,0.,-1.));
#16192=DIRECTION('center_axis',(0.,1.,0.));
#16193=DIRECTION('ref_axis',(1.,0.,0.));
#16194=DIRECTION('center_axis',(0.,-1.,0.));
#16195=DIRECTION('ref_axis',(1.,0.,0.));
#16196=DIRECTION('center_axis',(0.,-1.,0.));
#16197=DIRECTION('ref_axis',(0.,0.,-1.));
#16198=DIRECTION('center_axis',(0.,0.,1.));
#16199=DIRECTION('ref_axis',(1.,0.,0.));
#16200=DIRECTION('center_axis',(0.,-1.,0.));
#16201=DIRECTION('ref_axis',(0.,0.,-1.));
#16202=DIRECTION('center_axis',(0.,1.,0.));
#16203=DIRECTION('ref_axis',(1.,0.,0.));
#16204=DIRECTION('center_axis',(0.,-1.,0.));
#16205=DIRECTION('ref_axis',(1.,0.,0.));
#16206=DIRECTION('center_axis',(0.,-1.,0.));
#16207=DIRECTION('ref_axis',(0.,0.,-1.));
#16208=DIRECTION('center_axis',(6.12323399573676E-17,0.,1.));
#16209=DIRECTION('ref_axis',(1.,0.,0.));
#16210=DIRECTION('center_axis',(0.,-1.,0.));
#16211=DIRECTION('ref_axis',(0.,0.,-1.));
#16212=DIRECTION('center_axis',(0.,1.,0.));
#16213=DIRECTION('ref_axis',(1.,0.,0.));
#16214=DIRECTION('center_axis',(0.,-1.,0.));
#16215=DIRECTION('ref_axis',(1.,0.,0.));
#16216=DIRECTION('center_axis',(0.,-1.,0.));
#16217=DIRECTION('ref_axis',(0.,0.,-1.));
#16218=DIRECTION('center_axis',(0.,0.,1.));
#16219=DIRECTION('ref_axis',(1.,0.,0.));
#16220=DIRECTION('center_axis',(0.,-1.,0.));
#16221=DIRECTION('ref_axis',(0.,0.,-1.));
#16222=DIRECTION('center_axis',(0.,1.,0.));
#16223=DIRECTION('ref_axis',(1.,0.,0.));
#16224=DIRECTION('center_axis',(0.,1.,0.));
#16225=DIRECTION('ref_axis',(1.,0.,0.));
#16226=DIRECTION('',(0.,1.,0.));
#16227=DIRECTION('center_axis',(0.,-1.,0.));
#16228=DIRECTION('ref_axis',(1.,0.,0.));
#16229=DIRECTION('center_axis',(0.,-1.,0.));
#16230=DIRECTION('ref_axis',(1.,0.,0.));
#16231=DIRECTION('center_axis',(0.,1.,0.));
#16232=DIRECTION('ref_axis',(1.,0.,0.));
#16233=DIRECTION('center_axis',(0.,-1.,0.));
#16234=DIRECTION('ref_axis',(0.,0.,-1.));
#16235=DIRECTION('center_axis',(0.,0.,1.));
#16236=DIRECTION('ref_axis',(1.,0.,0.));
#16237=DIRECTION('center_axis',(0.,-1.,0.));
#16238=DIRECTION('ref_axis',(0.,0.,-1.));
#16239=DIRECTION('center_axis',(0.,-1.,0.));
#16240=DIRECTION('ref_axis',(-1.,0.,0.));
#16241=DIRECTION('center_axis',(0.,1.,0.));
#16242=DIRECTION('ref_axis',(1.,0.,0.));
#16243=DIRECTION('axis',(0.,0.,1.));
#16244=DIRECTION('refdir',(1.,0.,0.));
#16245=DIRECTION('center_axis',(0.,1.,0.));
#16246=DIRECTION('ref_axis',(0.,0.,1.));
#16247=DIRECTION('center_axis',(0.,-1.,0.));
#16248=DIRECTION('ref_axis',(1.,0.,0.));
#16249=DIRECTION('center_axis',(0.,-1.,0.));
#16250=DIRECTION('ref_axis',(1.,0.,0.));
#16251=DIRECTION('center_axis',(0.,-1.,0.));
#16252=DIRECTION('ref_axis',(1.,0.,0.));
#16253=DIRECTION('center_axis',(0.,-1.,0.));
#16254=DIRECTION('ref_axis',(1.,0.,0.));
#16255=DIRECTION('',(0.,1.,0.));
#16256=DIRECTION('center_axis',(0.,-1.,0.));
#16257=DIRECTION('ref_axis',(0.,0.,-1.));
#16258=DIRECTION('center_axis',(0.,-1.,0.));
#16259=DIRECTION('ref_axis',(1.,0.,0.));
#16260=DIRECTION('center_axis',(0.,-1.,0.));
#16261=DIRECTION('ref_axis',(1.,0.,0.));
#16262=DIRECTION('',(0.,1.,0.));
#16263=DIRECTION('center_axis',(0.,1.,0.));
#16264=DIRECTION('ref_axis',(0.,0.,1.));
#16265=DIRECTION('center_axis',(0.,-1.,0.));
#16266=DIRECTION('ref_axis',(1.,0.,0.));
#16267=DIRECTION('center_axis',(0.,-1.,0.));
#16268=DIRECTION('ref_axis',(1.,0.,0.));
#16269=DIRECTION('center_axis',(0.,-1.,0.));
#16270=DIRECTION('ref_axis',(1.,0.,0.));
#16271=DIRECTION('center_axis',(0.,-1.,0.));
#16272=DIRECTION('ref_axis',(1.,0.,0.));
#16273=DIRECTION('',(0.,1.,0.));
#16274=DIRECTION('center_axis',(0.,-1.,0.));
#16275=DIRECTION('ref_axis',(0.,0.,-1.));
#16276=DIRECTION('center_axis',(0.,-1.,0.));
#16277=DIRECTION('ref_axis',(1.,0.,0.));
#16278=DIRECTION('center_axis',(0.,-1.,0.));
#16279=DIRECTION('ref_axis',(1.,0.,0.));
#16280=DIRECTION('',(0.,1.,0.));
#16281=DIRECTION('',(0.,0.,1.));
#16282=DIRECTION('',(1.,0.,0.));
#16283=DIRECTION('',(0.,0.,1.));
#16284=DIRECTION('',(1.,0.,0.));
#16285=DIRECTION('',(0.,0.,1.));
#16286=DIRECTION('',(1.,0.,0.));
#16287=DIRECTION('',(0.,0.,1.));
#16288=DIRECTION('',(1.,0.,0.));
#16289=DIRECTION('',(0.,0.,1.));
#16290=DIRECTION('',(1.,0.,0.));
#16291=DIRECTION('axis',(0.,0.,1.));
#16292=DIRECTION('refdir',(1.,0.,0.));
#16293=DIRECTION('center_axis',(0.,0.,-1.));
#16294=DIRECTION('ref_axis',(0.,1.,0.));
#16295=DIRECTION('',(0.,1.,0.));
#16296=DIRECTION('',(1.,0.,0.));
#16297=DIRECTION('',(0.,-1.,0.));
#16298=DIRECTION('',(1.,0.,0.));
#16299=DIRECTION('center_axis',(0.,1.,-8.88178419700125E-16));
#16300=DIRECTION('ref_axis',(0.,8.88178419700125E-16,1.));
#16301=DIRECTION('',(0.,8.88178419700125E-16,1.));
#16302=DIRECTION('',(1.,0.,0.));
#16303=DIRECTION('',(0.,-8.88178419700125E-16,-1.));
#16304=DIRECTION('center_axis',(0.,-7.40148683083439E-16,-1.));
#16305=DIRECTION('ref_axis',(0.,1.,-7.40148683083439E-16));
#16306=DIRECTION('',(0.,1.,-7.40148683083439E-16));
#16307=DIRECTION('',(1.,0.,0.));
#16308=DIRECTION('',(0.,-1.,7.40148683083439E-16));
#16309=DIRECTION('center_axis',(0.,-0.707106781186547,-0.707106781186548));
#16310=DIRECTION('ref_axis',(0.,0.707106781186548,-0.707106781186547));
#16311=DIRECTION('',(0.,0.707106781186548,-0.707106781186547));
#16312=DIRECTION('',(1.,0.,0.));
#16313=DIRECTION('',(0.,-0.707106781186548,0.707106781186547));
#16314=DIRECTION('center_axis',(0.,-1.,2.77555756156289E-16));
#16315=DIRECTION('ref_axis',(0.,-2.77555756156289E-16,-1.));
#16316=DIRECTION('',(0.,-2.77555756156289E-16,-1.));
#16317=DIRECTION('',(1.,0.,0.));
#16318=DIRECTION('',(0.,2.77555756156289E-16,1.));
#16319=DIRECTION('center_axis',(0.,-0.707106781186547,0.707106781186548));
#16320=DIRECTION('ref_axis',(0.,-0.707106781186548,-0.707106781186547));
#16321=DIRECTION('',(0.,-0.707106781186548,-0.707106781186547));
#16322=DIRECTION('',(1.,0.,0.));
#16323=DIRECTION('',(0.,0.707106781186548,0.707106781186547));
#16324=DIRECTION('center_axis',(0.,7.40148683083438E-16,1.));
#16325=DIRECTION('ref_axis',(0.,-1.,7.40148683083438E-16));
#16326=DIRECTION('',(0.,-1.,7.40148683083438E-16));
#16327=DIRECTION('',(1.,0.,0.));
#16328=DIRECTION('',(0.,1.,-7.40148683083438E-16));
#16329=DIRECTION('center_axis',(0.,1.,-4.44089209850063E-16));
#16330=DIRECTION('ref_axis',(0.,4.44089209850063E-16,1.));
#16331=DIRECTION('',(0.,4.44089209850063E-16,1.));
#16332=DIRECTION('',(1.,0.,0.));
#16333=DIRECTION('',(0.,-4.44089209850063E-16,-1.));
#16334=DIRECTION('center_axis',(0.,2.41352831440251E-16,1.));
#16335=DIRECTION('ref_axis',(0.,-1.,2.41352831440251E-16));
#16336=DIRECTION('',(0.,-1.,2.41352831440251E-16));
#16337=DIRECTION('',(-1.,0.,0.));
#16338=DIRECTION('',(0.,1.,-2.41352831440251E-16));
#16339=DIRECTION('center_axis',(0.,-1.,2.41352831440251E-16));
#16340=DIRECTION('ref_axis',(0.,-2.41352831440251E-16,-1.));
#16341=DIRECTION('',(0.,-2.41352831440251E-16,-1.));
#16342=DIRECTION('',(1.,0.,0.));
#16343=DIRECTION('',(0.,2.41352831440251E-16,1.));
#16344=DIRECTION('',(1.,0.,0.));
#16345=DIRECTION('center_axis',(0.,0.,-1.));
#16346=DIRECTION('ref_axis',(0.,1.,0.));
#16347=DIRECTION('',(0.,1.,0.));
#16348=DIRECTION('',(1.,0.,0.));
#16349=DIRECTION('',(0.,-1.,0.));
#16350=DIRECTION('center_axis',(0.,-1.,0.));
#16351=DIRECTION('ref_axis',(0.,0.,-1.));
#16352=DIRECTION('',(0.,0.,-1.));
#16353=DIRECTION('',(1.,0.,0.));
#16354=DIRECTION('',(0.,0.,1.));
#16355=DIRECTION('center_axis',(0.,-0.707106781186547,0.707106781186548));
#16356=DIRECTION('ref_axis',(0.,-0.707106781186548,-0.707106781186547));
#16357=DIRECTION('',(0.,-0.707106781186548,-0.707106781186547));
#16358=DIRECTION('',(1.,0.,0.));
#16359=DIRECTION('',(0.,0.707106781186548,0.707106781186547));
#16360=DIRECTION('center_axis',(0.,0.,1.));
#16361=DIRECTION('ref_axis',(0.,-1.,0.));
#16362=DIRECTION('',(0.,-1.,0.));
#16363=DIRECTION('',(1.,0.,0.));
#16364=DIRECTION('',(0.,1.,0.));
#16365=DIRECTION('center_axis',(0.,0.707106781186548,0.707106781186547));
#16366=DIRECTION('ref_axis',(0.,-0.707106781186547,0.707106781186548));
#16367=DIRECTION('',(0.,-0.707106781186547,0.707106781186548));
#16368=DIRECTION('',(1.,0.,0.));
#16369=DIRECTION('',(0.,0.707106781186547,-0.707106781186548));
#16370=DIRECTION('center_axis',(0.,1.,0.));
#16371=DIRECTION('ref_axis',(0.,0.,1.));
#16372=DIRECTION('',(0.,0.,1.));
#16373=DIRECTION('',(1.,0.,0.));
#16374=DIRECTION('',(0.,0.,-1.));
#16375=DIRECTION('center_axis',(0.,0.,-1.));
#16376=DIRECTION('ref_axis',(0.,1.,0.));
#16377=DIRECTION('',(0.,1.,0.));
#16378=DIRECTION('',(1.,0.,0.));
#16379=DIRECTION('',(0.,-1.,0.));
#16380=DIRECTION('center_axis',(0.,1.,-2.41352831440251E-16));
#16381=DIRECTION('ref_axis',(0.,2.41352831440251E-16,1.));
#16382=DIRECTION('',(0.,2.41352831440251E-16,1.));
#16383=DIRECTION('',(-1.,0.,0.));
#16384=DIRECTION('',(0.,-2.41352831440251E-16,-1.));
#16385=DIRECTION('center_axis',(0.,0.,1.));
#16386=DIRECTION('ref_axis',(0.,-1.,0.));
#16387=DIRECTION('',(0.,-1.,0.));
#16388=DIRECTION('',(1.,0.,0.));
#16389=DIRECTION('',(0.,1.,0.));
#16390=DIRECTION('',(1.,0.,0.));
#16391=DIRECTION('center_axis',(0.,-1.,0.));
#16392=DIRECTION('ref_axis',(0.,0.,-1.));
#16393=DIRECTION('',(0.,0.,-1.));
#16394=DIRECTION('',(1.,0.,0.));
#16395=DIRECTION('',(0.,0.,1.));
#16396=DIRECTION('center_axis',(0.,0.,1.));
#16397=DIRECTION('ref_axis',(0.,-1.,0.));
#16398=DIRECTION('',(0.,-1.,0.));
#16399=DIRECTION('',(1.,0.,0.));
#16400=DIRECTION('',(0.,1.,0.));
#16401=DIRECTION('center_axis',(0.,0.707106781186548,0.707106781186548));
#16402=DIRECTION('ref_axis',(0.,-0.707106781186548,0.707106781186548));
#16403=DIRECTION('',(0.,-0.707106781186548,0.707106781186548));
#16404=DIRECTION('',(1.,0.,0.));
#16405=DIRECTION('',(0.,0.707106781186548,-0.707106781186548));
#16406=DIRECTION('center_axis',(0.,1.,0.));
#16407=DIRECTION('ref_axis',(0.,0.,1.));
#16408=DIRECTION('',(0.,0.,1.));
#16409=DIRECTION('',(1.,0.,0.));
#16410=DIRECTION('',(0.,0.,-1.));
#16411=DIRECTION('center_axis',(0.,0.707106781186548,-0.707106781186547));
#16412=DIRECTION('ref_axis',(0.,0.707106781186547,0.707106781186548));
#16413=DIRECTION('',(0.,0.707106781186547,0.707106781186548));
#16414=DIRECTION('',(1.,0.,0.));
#16415=DIRECTION('',(0.,-0.707106781186547,-0.707106781186548));
#16416=DIRECTION('center_axis',(0.,-7.40148683083438E-16,-1.));
#16417=DIRECTION('ref_axis',(0.,1.,-7.40148683083438E-16));
#16418=DIRECTION('',(0.,1.,-7.40148683083438E-16));
#16419=DIRECTION('',(1.,0.,0.));
#16420=DIRECTION('',(0.,-1.,7.40148683083438E-16));
#16421=DIRECTION('center_axis',(0.,-1.,0.));
#16422=DIRECTION('ref_axis',(0.,0.,-1.));
#16423=DIRECTION('',(0.,0.,-1.));
#16424=DIRECTION('',(1.,0.,0.));
#16425=DIRECTION('',(0.,0.,1.));
#16426=DIRECTION('center_axis',(0.,0.,-1.));
#16427=DIRECTION('ref_axis',(0.,1.,0.));
#16428=DIRECTION('',(0.,1.,0.));
#16429=DIRECTION('',(-1.,0.,0.));
#16430=DIRECTION('',(0.,-1.,0.));
#16431=DIRECTION('center_axis',(0.,1.,0.));
#16432=DIRECTION('ref_axis',(0.,0.,1.));
#16433=DIRECTION('',(0.,0.,1.));
#16434=DIRECTION('',(1.,0.,0.));
#16435=DIRECTION('',(0.,0.,-1.));
#16436=DIRECTION('',(1.,0.,0.));
#16437=DIRECTION('center_axis',(0.,0.,1.));
#16438=DIRECTION('ref_axis',(0.,-1.,0.));
#16439=DIRECTION('',(0.,-1.,0.));
#16440=DIRECTION('',(1.,0.,0.));
#16441=DIRECTION('',(0.,1.,0.));
#16442=DIRECTION('center_axis',(0.,1.,0.));
#16443=DIRECTION('ref_axis',(0.,0.,1.));
#16444=DIRECTION('',(0.,0.,1.));
#16445=DIRECTION('',(1.,0.,0.));
#16446=DIRECTION('',(0.,0.,-1.));
#16447=DIRECTION('center_axis',(0.,0.707106781186547,-0.707106781186548));
#16448=DIRECTION('ref_axis',(0.,0.707106781186548,0.707106781186547));
#16449=DIRECTION('',(0.,0.707106781186548,0.707106781186547));
#16450=DIRECTION('',(1.,0.,0.));
#16451=DIRECTION('',(0.,-0.707106781186548,-0.707106781186547));
#16452=DIRECTION('center_axis',(0.,0.,-1.));
#16453=DIRECTION('ref_axis',(0.,1.,0.));
#16454=DIRECTION('',(0.,1.,0.));
#16455=DIRECTION('',(1.,0.,0.));
#16456=DIRECTION('',(0.,-1.,0.));
#16457=DIRECTION('center_axis',(0.,-0.707106781186547,-0.707106781186548));
#16458=DIRECTION('ref_axis',(0.,0.707106781186548,-0.707106781186547));
#16459=DIRECTION('',(0.,0.707106781186548,-0.707106781186547));
#16460=DIRECTION('',(1.,0.,0.));
#16461=DIRECTION('',(0.,-0.707106781186548,0.707106781186547));
#16462=DIRECTION('center_axis',(0.,-1.,0.));
#16463=DIRECTION('ref_axis',(0.,0.,-1.));
#16464=DIRECTION('',(0.,0.,-1.));
#16465=DIRECTION('',(1.,0.,0.));
#16466=DIRECTION('',(0.,0.,1.));
#16467=DIRECTION('center_axis',(0.,0.,1.));
#16468=DIRECTION('ref_axis',(0.,-1.,0.));
#16469=DIRECTION('',(0.,-1.,0.));
#16470=DIRECTION('',(1.,0.,0.));
#16471=DIRECTION('',(0.,1.,0.));
#16472=DIRECTION('center_axis',(0.,-1.,0.));
#16473=DIRECTION('ref_axis',(0.,0.,-1.));
#16474=DIRECTION('',(0.,0.,-1.));
#16475=DIRECTION('',(-1.,0.,0.));
#16476=DIRECTION('',(0.,0.,1.));
#16477=DIRECTION('center_axis',(1.,0.,0.));
#16478=DIRECTION('ref_axis',(0.,0.,-1.));
#16479=DIRECTION('center_axis',(1.,0.,0.));
#16480=DIRECTION('ref_axis',(0.,0.,-1.));
#16481=DIRECTION('',(1.,0.,0.));
#16482=DIRECTION('center_axis',(-1.,0.,0.));
#16483=DIRECTION('ref_axis',(0.,0.,-1.));
#16484=DIRECTION('center_axis',(0.,1.,0.));
#16485=DIRECTION('ref_axis',(0.,0.,1.));
#16486=DIRECTION('',(0.,0.,1.));
#16487=DIRECTION('',(1.,0.,0.));
#16488=DIRECTION('',(0.,0.,1.));
#16489=DIRECTION('center_axis',(0.,1.,0.));
#16490=DIRECTION('ref_axis',(0.,0.,1.));
#16491=DIRECTION('',(0.,0.,1.));
#16492=DIRECTION('',(1.,0.,0.));
#16493=DIRECTION('',(0.,0.,1.));
#16494=DIRECTION('center_axis',(0.,0.,-1.));
#16495=DIRECTION('ref_axis',(0.,1.,0.));
#16496=DIRECTION('',(0.,1.,0.));
#16497=DIRECTION('',(0.,1.,0.));
#16498=DIRECTION('center_axis',(0.,0.,-1.));
#16499=DIRECTION('ref_axis',(0.,1.,0.));
#16500=DIRECTION('',(0.,1.,0.));
#16501=DIRECTION('',(1.,0.,0.));
#16502=DIRECTION('',(0.,1.,0.));
#16503=DIRECTION('center_axis',(0.,-1.,0.));
#16504=DIRECTION('ref_axis',(0.,0.,-1.));
#16505=DIRECTION('',(0.,0.,-1.));
#16506=DIRECTION('',(0.,0.,-1.));
#16507=DIRECTION('center_axis',(0.,-1.,0.));
#16508=DIRECTION('ref_axis',(0.,0.,-1.));
#16509=DIRECTION('',(0.,0.,-1.));
#16510=DIRECTION('',(1.,0.,0.));
#16511=DIRECTION('',(0.,0.,-1.));
#16512=DIRECTION('center_axis',(0.,0.,1.));
#16513=DIRECTION('ref_axis',(0.,-1.,0.));
#16514=DIRECTION('',(0.,-1.,0.));
#16515=DIRECTION('',(0.,-1.,0.));
#16516=DIRECTION('center_axis',(0.,0.,1.));
#16517=DIRECTION('ref_axis',(0.,-1.,0.));
#16518=DIRECTION('',(0.,-1.,0.));
#16519=DIRECTION('',(0.,-1.,0.));
#16520=DIRECTION('center_axis',(1.,0.,0.));
#16521=DIRECTION('ref_axis',(0.,0.,-1.));
#16522=DIRECTION('center_axis',(1.,0.,0.));
#16523=DIRECTION('ref_axis',(0.,0.,-1.));
#16524=DIRECTION('axis',(0.,0.,1.));
#16525=DIRECTION('refdir',(1.,0.,0.));
#16526=DIRECTION('center_axis',(0.,-0.707106781186548,-0.707106781186548));
#16527=DIRECTION('ref_axis',(-1.,0.,0.));
#16528=DIRECTION('',(0.,-0.707106781186548,0.707106781186548));
#16529=DIRECTION('',(-1.,0.,0.));
#16530=DIRECTION('',(0.,0.707106781186548,-0.707106781186548));
#16531=DIRECTION('',(1.,0.,0.));
#16532=DIRECTION('center_axis',(0.,0.707106781186548,0.707106781186548));
#16533=DIRECTION('ref_axis',(0.,0.707106781186547,-0.707106781186547));
#16534=DIRECTION('',(1.,0.,0.));
#16535=DIRECTION('center_axis',(0.,0.,1.));
#16536=DIRECTION('ref_axis',(1.,0.,0.));
#16537=DIRECTION('center_axis',(0.,0.,-1.));
#16538=DIRECTION('ref_axis',(1.,0.,0.));
#16539=DIRECTION('',(0.,0.,1.));
#16540=DIRECTION('center_axis',(0.,0.,-1.));
#16541=DIRECTION('ref_axis',(1.,0.,0.));
#16542=DIRECTION('center_axis',(0.,0.,-1.));
#16543=DIRECTION('ref_axis',(1.,0.,0.));
#16544=DIRECTION('center_axis',(0.,-0.707106781186548,0.707106781186548));
#16545=DIRECTION('ref_axis',(0.,0.707106781186547,0.707106781186547));
#16546=DIRECTION('center_axis',(0.,0.,-1.));
#16547=DIRECTION('ref_axis',(1.,0.,0.));
#16548=DIRECTION('center_axis',(0.,0.,1.));
#16549=DIRECTION('ref_axis',(1.,0.,0.));
#16550=DIRECTION('',(0.,-1.,0.));
#16551=DIRECTION('',(-1.,0.,0.));
#16552=DIRECTION('center_axis',(0.,0.,1.));
#16553=DIRECTION('ref_axis',(1.,0.,0.));
#16554=DIRECTION('',(-1.,0.,0.));
#16555=DIRECTION('',(0.,1.,0.));
#16556=DIRECTION('center_axis',(0.,0.707106781186548,-0.707106781186548));
#16557=DIRECTION('ref_axis',(-1.,0.,0.));
#16558=DIRECTION('',(0.,0.707106781186548,0.707106781186548));
#16559=DIRECTION('',(1.,0.,0.));
#16560=DIRECTION('',(0.,-0.707106781186548,-0.707106781186548));
#16561=DIRECTION('center_axis',(1.,0.,0.));
#16562=DIRECTION('ref_axis',(0.,1.,0.));
#16563=DIRECTION('',(0.,0.,1.));
#16564=DIRECTION('',(0.,1.,0.));
#16565=DIRECTION('',(0.,0.,1.));
#16566=DIRECTION('center_axis',(0.,1.,0.));
#16567=DIRECTION('ref_axis',(-1.,0.,0.));
#16568=DIRECTION('',(0.,0.,1.));
#16569=DIRECTION('',(-1.,0.,0.));
#16570=DIRECTION('center_axis',(0.,-1.,0.));
#16571=DIRECTION('ref_axis',(1.,0.,0.));
#16572=DIRECTION('',(1.,0.,0.));
#16573=DIRECTION('',(0.,0.,1.));
#16574=DIRECTION('center_axis',(-1.,0.,0.));
#16575=DIRECTION('ref_axis',(0.,-1.,0.));
#16576=DIRECTION('',(0.,-1.,0.));
#16577=DIRECTION('center_axis',(0.,0.,1.));
#16578=DIRECTION('ref_axis',(1.,0.,0.));
#16579=DIRECTION('axis',(0.,0.,1.));
#16580=DIRECTION('refdir',(1.,0.,0.));
#16581=DIRECTION('center_axis',(0.,1.,0.));
#16582=DIRECTION('ref_axis',(1.,0.,0.));
#16583=DIRECTION('center_axis',(0.,1.,0.));
#16584=DIRECTION('ref_axis',(1.,0.,0.));
#16585=DIRECTION('',(0.707106781186548,-0.707106781186547,-8.65956056235494E-17));
#16586=DIRECTION('center_axis',(0.,-1.,0.));
#16587=DIRECTION('ref_axis',(1.,0.,0.));
#16588=DIRECTION('center_axis',(0.,1.,0.));
#16589=DIRECTION('ref_axis',(1.,0.,0.));
#16590=DIRECTION('',(0.,-1.,0.));
#16591=DIRECTION('center_axis',(0.,-1.,0.));
#16592=DIRECTION('ref_axis',(1.,0.,0.));
#16593=DIRECTION('center_axis',(0.,1.,0.));
#16594=DIRECTION('ref_axis',(1.,0.,0.));
#16595=DIRECTION('center_axis',(0.,1.,0.));
#16596=DIRECTION('ref_axis',(1.,0.,0.));
#16597=DIRECTION('center_axis',(0.,1.,0.));
#16598=DIRECTION('ref_axis',(1.,0.,0.));
#16599=DIRECTION('',(0.,-1.,0.));
#16600=DIRECTION('center_axis',(0.,1.,0.));
#16601=DIRECTION('ref_axis',(1.,0.,0.));
#16602=DIRECTION('center_axis',(0.,1.,0.));
#16603=DIRECTION('ref_axis',(1.,0.,0.));
#16604=DIRECTION('axis',(0.,0.,1.));
#16605=DIRECTION('refdir',(1.,0.,0.));
#16606=DIRECTION('center_axis',(0.866025403784439,0.,-0.5));
#16607=DIRECTION('ref_axis',(0.5,0.,0.866025403784439));
#16608=DIRECTION('',(-0.5,0.,-0.866025403784439));
#16609=DIRECTION('',(0.,-1.,0.));
#16610=DIRECTION('',(0.5,0.,0.866025403784439));
#16611=DIRECTION('',(0.,-1.,0.));
#16612=DIRECTION('center_axis',(1.20185167898973E-16,0.,-1.));
#16613=DIRECTION('ref_axis',(1.,0.,1.20185167898973E-16));
#16614=DIRECTION('',(-1.,0.,-1.20185167898973E-16));
#16615=DIRECTION('',(0.,-1.,0.));
#16616=DIRECTION('',(1.,0.,1.20185167898973E-16));
#16617=DIRECTION('center_axis',(-0.866025403784439,0.,-0.5));
#16618=DIRECTION('ref_axis',(0.5,0.,-0.866025403784439));
#16619=DIRECTION('',(-0.5,0.,0.866025403784439));
#16620=DIRECTION('',(0.,-1.,0.));
#16621=DIRECTION('',(0.5,0.,-0.866025403784439));
#16622=DIRECTION('center_axis',(-0.866025403784439,0.,0.5));
#16623=DIRECTION('ref_axis',(-0.5,0.,-0.866025403784439));
#16624=DIRECTION('',(0.5,0.,0.866025403784439));
#16625=DIRECTION('',(0.,-1.,0.));
#16626=DIRECTION('',(-0.5,0.,-0.866025403784439));
#16627=DIRECTION('center_axis',(-2.40370335797945E-16,0.,1.));
#16628=DIRECTION('ref_axis',(-1.,0.,-2.40370335797945E-16));
#16629=DIRECTION('',(1.,0.,2.40370335797945E-16));
#16630=DIRECTION('',(0.,-1.,0.));
#16631=DIRECTION('',(-1.,0.,-2.40370335797945E-16));
#16632=DIRECTION('center_axis',(0.866025403784439,0.,0.5));
#16633=DIRECTION('ref_axis',(-0.5,0.,0.866025403784439));
#16634=DIRECTION('',(0.5,0.,-0.866025403784439));
#16635=DIRECTION('',(-0.5,0.,0.866025403784439));
#16636=DIRECTION('center_axis',(0.,1.,0.));
#16637=DIRECTION('ref_axis',(1.,0.,0.));
#16638=DIRECTION('center_axis',(0.,-1.,0.));
#16639=DIRECTION('ref_axis',(0.,0.,-1.));
#16640=DIRECTION('center_axis',(0.,1.,0.));
#16641=DIRECTION('ref_axis',(1.,0.,0.));
#16642=DIRECTION('center_axis',(0.,1.,0.));
#16643=DIRECTION('ref_axis',(1.,0.,0.));
#16644=DIRECTION('center_axis',(0.,1.,0.));
#16645=DIRECTION('ref_axis',(0.,0.,1.));
#16646=DIRECTION('center_axis',(0.,-1.,0.));
#16647=DIRECTION('ref_axis',(1.,0.,0.));
#16648=DIRECTION('center_axis',(0.,-1.,0.));
#16649=DIRECTION('ref_axis',(1.,0.,0.));
#16650=DIRECTION('center_axis',(0.,-1.,0.));
#16651=DIRECTION('ref_axis',(1.,0.,0.));
#16652=DIRECTION('',(0.707106781186548,0.707106781186547,8.65956056235493E-17));
#16653=DIRECTION('center_axis',(0.,-1.,0.));
#16654=DIRECTION('ref_axis',(1.,0.,0.));
#16655=DIRECTION('center_axis',(0.,-1.,0.));
#16656=DIRECTION('ref_axis',(1.,0.,0.));
#16657=DIRECTION('',(0.,1.,0.));
#16658=DIRECTION('center_axis',(0.,1.,0.));
#16659=DIRECTION('ref_axis',(1.,0.,0.));
#16660=DIRECTION('center_axis',(0.,-1.,0.));
#16661=DIRECTION('ref_axis',(1.,0.,0.));
#16662=DIRECTION('',(-0.707106781186547,0.707106781186548,-8.65956056235493E-17));
#16663=DIRECTION('center_axis',(0.,-1.,0.));
#16664=DIRECTION('ref_axis',(0.,0.,-1.));
#16665=DIRECTION('center_axis',(0.,-1.,0.));
#16666=DIRECTION('ref_axis',(1.,0.,0.));
#16667=DIRECTION('center_axis',(0.,1.,0.));
#16668=DIRECTION('ref_axis',(1.,0.,0.));
#16669=DIRECTION('center_axis',(0.,1.,0.));
#16670=DIRECTION('ref_axis',(1.,0.,0.));
#16671=DIRECTION('',(-0.447213595499958,0.894427190999916,-5.47678698264203E-17));
#16672=DIRECTION('center_axis',(0.,-1.,0.));
#16673=DIRECTION('ref_axis',(1.,0.,0.));
#16674=DIRECTION('',(0.,1.,0.));
#16675=DIRECTION('axis',(0.,0.,1.));
#16676=DIRECTION('refdir',(1.,0.,0.));
#16677=DIRECTION('axis',(0.,0.,1.));
#16678=DIRECTION('refdir',(1.,0.,0.));
#16679=DIRECTION('center_axis',(0.,0.,1.));
#16680=DIRECTION('ref_axis',(1.,0.,0.));
#16681=DIRECTION('center_axis',(0.,0.,1.));
#16682=DIRECTION('ref_axis',(1.,0.,0.));
#16683=DIRECTION('',(0.,0.,1.));
#16684=DIRECTION('center_axis',(0.,0.,-1.));
#16685=DIRECTION('ref_axis',(1.,0.,0.));
#16686=DIRECTION('center_axis',(0.,0.,1.));
#16687=DIRECTION('ref_axis',(1.,0.,0.));
#16688=DIRECTION('center_axis',(0.,0.,1.));
#16689=DIRECTION('ref_axis',(1.,0.,0.));
#16690=DIRECTION('',(0.,0.,1.));
#16691=DIRECTION('center_axis',(0.,0.,-1.));
#16692=DIRECTION('ref_axis',(1.,0.,0.));
#16693=DIRECTION('center_axis',(0.,0.,1.));
#16694=DIRECTION('ref_axis',(1.,0.,0.));
#16695=DIRECTION('center_axis',(0.,0.,1.));
#16696=DIRECTION('ref_axis',(1.,0.,0.));
#16697=DIRECTION('',(0.,0.,1.));
#16698=DIRECTION('center_axis',(0.,0.,-1.));
#16699=DIRECTION('ref_axis',(1.,0.,0.));
#16700=DIRECTION('center_axis',(0.,0.,1.));
#16701=DIRECTION('ref_axis',(1.,0.,0.));
#16702=DIRECTION('center_axis',(0.,0.,1.));
#16703=DIRECTION('ref_axis',(1.,0.,0.));
#16704=DIRECTION('',(0.,0.,1.));
#16705=DIRECTION('center_axis',(0.,0.,-1.));
#16706=DIRECTION('ref_axis',(1.,0.,0.));
#16707=DIRECTION('center_axis',(0.,1.,0.));
#16708=DIRECTION('ref_axis',(-1.,0.,0.));
#16709=DIRECTION('',(-1.,0.,0.));
#16710=DIRECTION('',(0.,0.,1.));
#16711=DIRECTION('',(-1.,0.,0.));
#16712=DIRECTION('',(0.,0.,1.));
#16713=DIRECTION('center_axis',(1.,0.,0.));
#16714=DIRECTION('ref_axis',(0.,1.,0.));
#16715=DIRECTION('',(0.,1.,0.));
#16716=DIRECTION('',(0.,1.,0.));
#16717=DIRECTION('',(0.,0.,1.));
#16718=DIRECTION('center_axis',(0.,-1.,0.));
#16719=DIRECTION('ref_axis',(1.,0.,0.));
#16720=DIRECTION('',(1.,0.,0.));
#16721=DIRECTION('',(1.,0.,0.));
#16722=DIRECTION('',(0.,0.,1.));
#16723=DIRECTION('center_axis',(-1.,0.,0.));
#16724=DIRECTION('ref_axis',(0.,-1.,0.));
#16725=DIRECTION('',(0.,-1.,0.));
#16726=DIRECTION('',(0.,-1.,0.));
#16727=DIRECTION('center_axis',(0.,0.,1.));
#16728=DIRECTION('ref_axis',(1.,0.,0.));
#16729=DIRECTION('center_axis',(0.,0.,1.));
#16730=DIRECTION('ref_axis',(1.,0.,0.));
#16731=DIRECTION('axis',(0.,0.,1.));
#16732=DIRECTION('refdir',(1.,0.,0.));
#16733=DIRECTION('center_axis',(0.,0.,1.));
#16734=DIRECTION('ref_axis',(1.,0.,0.));
#16735=DIRECTION('center_axis',(0.,0.,1.));
#16736=DIRECTION('ref_axis',(1.,0.,0.));
#16737=DIRECTION('',(0.,0.,1.));
#16738=DIRECTION('center_axis',(0.,0.,-1.));
#16739=DIRECTION('ref_axis',(1.,0.,0.));
#16740=DIRECTION('center_axis',(0.,0.,1.));
#16741=DIRECTION('ref_axis',(1.,0.,0.));
#16742=DIRECTION('center_axis',(0.,0.,1.));
#16743=DIRECTION('ref_axis',(1.,0.,0.));
#16744=DIRECTION('',(0.,0.,1.));
#16745=DIRECTION('center_axis',(0.,0.,-1.));
#16746=DIRECTION('ref_axis',(1.,0.,0.));
#16747=DIRECTION('center_axis',(0.,0.,1.));
#16748=DIRECTION('ref_axis',(1.,0.,0.));
#16749=DIRECTION('center_axis',(0.,0.,1.));
#16750=DIRECTION('ref_axis',(1.,0.,0.));
#16751=DIRECTION('',(0.,0.,1.));
#16752=DIRECTION('center_axis',(0.,0.,-1.));
#16753=DIRECTION('ref_axis',(1.,0.,0.));
#16754=DIRECTION('center_axis',(0.,0.,1.));
#16755=DIRECTION('ref_axis',(1.,0.,0.));
#16756=DIRECTION('center_axis',(0.,0.,1.));
#16757=DIRECTION('ref_axis',(1.,0.,0.));
#16758=DIRECTION('',(0.,0.,1.));
#16759=DIRECTION('center_axis',(0.,0.,-1.));
#16760=DIRECTION('ref_axis',(1.,0.,0.));
#16761=DIRECTION('center_axis',(0.,0.,1.));
#16762=DIRECTION('ref_axis',(1.,0.,0.));
#16763=DIRECTION('center_axis',(0.,0.,1.));
#16764=DIRECTION('ref_axis',(1.,0.,0.));
#16765=DIRECTION('',(0.,0.,1.));
#16766=DIRECTION('center_axis',(0.,0.,-1.));
#16767=DIRECTION('ref_axis',(1.,0.,0.));
#16768=DIRECTION('center_axis',(0.,0.,1.));
#16769=DIRECTION('ref_axis',(1.,0.,0.));
#16770=DIRECTION('center_axis',(0.,0.,1.));
#16771=DIRECTION('ref_axis',(1.,0.,0.));
#16772=DIRECTION('',(0.,0.,1.));
#16773=DIRECTION('center_axis',(0.,0.,-1.));
#16774=DIRECTION('ref_axis',(1.,0.,0.));
#16775=DIRECTION('center_axis',(0.,0.,1.));
#16776=DIRECTION('ref_axis',(1.,0.,0.));
#16777=DIRECTION('center_axis',(0.,0.,1.));
#16778=DIRECTION('ref_axis',(1.,0.,0.));
#16779=DIRECTION('',(0.,0.,1.));
#16780=DIRECTION('center_axis',(0.,0.,-1.));
#16781=DIRECTION('ref_axis',(1.,0.,0.));
#16782=DIRECTION('center_axis',(0.,0.,1.));
#16783=DIRECTION('ref_axis',(1.,0.,0.));
#16784=DIRECTION('center_axis',(0.,0.,1.));
#16785=DIRECTION('ref_axis',(1.,0.,0.));
#16786=DIRECTION('',(0.,0.,1.));
#16787=DIRECTION('center_axis',(0.,0.,-1.));
#16788=DIRECTION('ref_axis',(1.,0.,0.));
#16789=DIRECTION('center_axis',(0.,1.,0.));
#16790=DIRECTION('ref_axis',(-1.,0.,0.));
#16791=DIRECTION('',(-1.,0.,0.));
#16792=DIRECTION('',(0.,0.,1.));
#16793=DIRECTION('',(-1.,0.,0.));
#16794=DIRECTION('',(0.,0.,1.));
#16795=DIRECTION('center_axis',(1.,0.,0.));
#16796=DIRECTION('ref_axis',(0.,1.,0.));
#16797=DIRECTION('',(0.,1.,0.));
#16798=DIRECTION('',(0.,1.,0.));
#16799=DIRECTION('',(0.,0.,1.));
#16800=DIRECTION('center_axis',(0.,-1.,0.));
#16801=DIRECTION('ref_axis',(1.,0.,0.));
#16802=DIRECTION('',(1.,0.,0.));
#16803=DIRECTION('',(1.,0.,0.));
#16804=DIRECTION('',(0.,0.,1.));
#16805=DIRECTION('center_axis',(-1.,0.,0.));
#16806=DIRECTION('ref_axis',(0.,-1.,0.));
#16807=DIRECTION('',(0.,-1.,0.));
#16808=DIRECTION('',(0.,-1.,0.));
#16809=DIRECTION('center_axis',(0.,0.,1.));
#16810=DIRECTION('ref_axis',(1.,0.,0.));
#16811=DIRECTION('center_axis',(0.,0.,1.));
#16812=DIRECTION('ref_axis',(1.,0.,0.));
#16813=DIRECTION('axis',(0.,0.,1.));
#16814=DIRECTION('refdir',(1.,0.,0.));
#16815=DIRECTION('center_axis',(0.,0.,1.));
#16816=DIRECTION('ref_axis',(1.,0.,0.));
#16817=DIRECTION('center_axis',(0.,0.,1.));
#16818=DIRECTION('ref_axis',(1.,0.,0.));
#16819=DIRECTION('',(0.,0.,1.));
#16820=DIRECTION('center_axis',(0.,0.,-1.));
#16821=DIRECTION('ref_axis',(1.,0.,0.));
#16822=DIRECTION('center_axis',(0.,0.,1.));
#16823=DIRECTION('ref_axis',(1.,0.,0.));
#16824=DIRECTION('center_axis',(0.,0.,1.));
#16825=DIRECTION('ref_axis',(1.,0.,0.));
#16826=DIRECTION('center_axis',(0.,0.,1.));
#16827=DIRECTION('ref_axis',(1.,0.,0.));
#16828=DIRECTION('',(0.,0.,1.));
#16829=DIRECTION('center_axis',(0.,0.,-1.));
#16830=DIRECTION('ref_axis',(1.,0.,0.));
#16831=DIRECTION('center_axis',(0.,0.,1.));
#16832=DIRECTION('ref_axis',(1.,0.,0.));
#16833=DIRECTION('center_axis',(0.,0.,1.));
#16834=DIRECTION('ref_axis',(1.,0.,0.));
#16835=DIRECTION('center_axis',(0.,0.,1.));
#16836=DIRECTION('ref_axis',(1.,0.,0.));
#16837=DIRECTION('',(0.,0.,1.));
#16838=DIRECTION('center_axis',(0.,0.,-1.));
#16839=DIRECTION('ref_axis',(1.,0.,0.));
#16840=DIRECTION('center_axis',(0.,0.,1.));
#16841=DIRECTION('ref_axis',(1.,0.,0.));
#16842=DIRECTION('center_axis',(0.,0.,1.));
#16843=DIRECTION('ref_axis',(1.,0.,0.));
#16844=DIRECTION('center_axis',(0.,0.,1.));
#16845=DIRECTION('ref_axis',(1.,0.,0.));
#16846=DIRECTION('',(0.,0.,1.));
#16847=DIRECTION('center_axis',(0.,0.,-1.));
#16848=DIRECTION('ref_axis',(1.,0.,0.));
#16849=DIRECTION('center_axis',(0.,0.,1.));
#16850=DIRECTION('ref_axis',(1.,0.,0.));
#16851=DIRECTION('center_axis',(1.,0.,0.));
#16852=DIRECTION('ref_axis',(0.,0.,-1.));
#16853=DIRECTION('center_axis',(1.,0.,0.));
#16854=DIRECTION('ref_axis',(0.,0.,-1.));
#16855=DIRECTION('',(1.,0.,0.));
#16856=DIRECTION('center_axis',(-1.,0.,0.));
#16857=DIRECTION('ref_axis',(0.,0.,-1.));
#16858=DIRECTION('center_axis',(1.,0.,0.));
#16859=DIRECTION('ref_axis',(0.,0.,-1.));
#16860=DIRECTION('center_axis',(1.,0.,0.));
#16861=DIRECTION('ref_axis',(0.,0.,-1.));
#16862=DIRECTION('center_axis',(1.,0.,0.));
#16863=DIRECTION('ref_axis',(0.,0.,-1.));
#16864=DIRECTION('',(1.,0.,0.));
#16865=DIRECTION('center_axis',(-1.,0.,0.));
#16866=DIRECTION('ref_axis',(0.,0.,-1.));
#16867=DIRECTION('center_axis',(1.,0.,0.));
#16868=DIRECTION('ref_axis',(0.,0.,-1.));
#16869=DIRECTION('center_axis',(1.,0.,0.));
#16870=DIRECTION('ref_axis',(0.,0.,-1.));
#16871=DIRECTION('center_axis',(1.,0.,0.));
#16872=DIRECTION('ref_axis',(0.,0.,-1.));
#16873=DIRECTION('',(1.,0.,0.));
#16874=DIRECTION('center_axis',(-1.,0.,0.));
#16875=DIRECTION('ref_axis',(0.,0.,-1.));
#16876=DIRECTION('center_axis',(1.,0.,0.));
#16877=DIRECTION('ref_axis',(0.,0.,-1.));
#16878=DIRECTION('center_axis',(1.,0.,0.));
#16879=DIRECTION('ref_axis',(0.,0.,-1.));
#16880=DIRECTION('center_axis',(1.,0.,0.));
#16881=DIRECTION('ref_axis',(0.,0.,-1.));
#16882=DIRECTION('',(1.,0.,0.));
#16883=DIRECTION('center_axis',(-1.,0.,0.));
#16884=DIRECTION('ref_axis',(0.,0.,-1.));
#16885=DIRECTION('center_axis',(0.,1.,0.));
#16886=DIRECTION('ref_axis',(-1.,0.,0.));
#16887=DIRECTION('',(-1.,0.,0.));
#16888=DIRECTION('',(0.,0.,1.));
#16889=DIRECTION('',(-1.,0.,0.));
#16890=DIRECTION('',(0.,0.,1.));
#16891=DIRECTION('center_axis',(1.,0.,0.));
#16892=DIRECTION('ref_axis',(0.,1.,0.));
#16893=DIRECTION('',(0.,1.,0.));
#16894=DIRECTION('',(0.,1.,0.));
#16895=DIRECTION('',(0.,0.,1.));
#16896=DIRECTION('center_axis',(0.,-1.,0.));
#16897=DIRECTION('ref_axis',(1.,0.,0.));
#16898=DIRECTION('',(1.,0.,0.));
#16899=DIRECTION('',(1.,0.,0.));
#16900=DIRECTION('',(0.,0.,1.));
#16901=DIRECTION('center_axis',(-1.,0.,0.));
#16902=DIRECTION('ref_axis',(0.,-1.,0.));
#16903=DIRECTION('',(0.,-1.,0.));
#16904=DIRECTION('',(0.,-1.,0.));
#16905=DIRECTION('center_axis',(0.,0.,1.));
#16906=DIRECTION('ref_axis',(1.,0.,0.));
#16907=DIRECTION('center_axis',(0.,0.,1.));
#16908=DIRECTION('ref_axis',(1.,0.,0.));
#16909=DIRECTION('axis',(0.,0.,1.));
#16910=DIRECTION('refdir',(1.,0.,0.));
#16911=DIRECTION('axis',(0.,0.,1.));
#16912=DIRECTION('refdir',(1.,0.,0.));
#16913=DIRECTION('center_axis',(0.,0.,1.));
#16914=DIRECTION('ref_axis',(1.,0.,0.));
#16915=DIRECTION('',(-1.,0.,0.));
#16916=DIRECTION('center_axis',(0.,0.,1.));
#16917=DIRECTION('ref_axis',(1.,0.,0.));
#16918=DIRECTION('center_axis',(0.,0.,1.));
#16919=DIRECTION('ref_axis',(1.,0.,0.));
#16920=DIRECTION('',(0.,0.,-1.));
#16921=DIRECTION('center_axis',(0.,0.,1.));
#16922=DIRECTION('ref_axis',(1.,0.,0.));
#16923=DIRECTION('',(0.,0.,1.));
#16924=DIRECTION('center_axis',(0.,0.,-1.));
#16925=DIRECTION('ref_axis',(1.,0.,0.));
#16926=DIRECTION('center_axis',(0.,0.,1.));
#16927=DIRECTION('ref_axis',(1.,0.,0.));
#16928=DIRECTION('',(0.,0.,1.));
#16929=DIRECTION('center_axis',(0.,0.,1.));
#16930=DIRECTION('ref_axis',(1.,0.,0.));
#16931=DIRECTION('',(1.,0.,0.));
#16932=DIRECTION('center_axis',(0.,0.,1.));
#16933=DIRECTION('ref_axis',(1.,0.,0.));
#16934=DIRECTION('center_axis',(0.,0.,1.));
#16935=DIRECTION('ref_axis',(1.,0.,0.));
#16936=DIRECTION('',(0.,0.,-1.));
#16937=DIRECTION('center_axis',(0.,0.,1.));
#16938=DIRECTION('ref_axis',(1.,0.,0.));
#16939=DIRECTION('',(0.,0.,1.));
#16940=DIRECTION('center_axis',(0.,0.,-1.));
#16941=DIRECTION('ref_axis',(1.,0.,0.));
#16942=DIRECTION('center_axis',(0.,0.,1.));
#16943=DIRECTION('ref_axis',(1.,0.,0.));
#16944=DIRECTION('',(0.,0.,1.));
#16945=DIRECTION('center_axis',(0.,0.,1.));
#16946=DIRECTION('ref_axis',(1.,0.,0.));
#16947=DIRECTION('',(-1.,0.,0.));
#16948=DIRECTION('center_axis',(0.,0.,1.));
#16949=DIRECTION('ref_axis',(1.,0.,0.));
#16950=DIRECTION('center_axis',(0.,0.,1.));
#16951=DIRECTION('ref_axis',(1.,0.,0.));
#16952=DIRECTION('',(0.,0.,-1.));
#16953=DIRECTION('center_axis',(0.,0.,1.));
#16954=DIRECTION('ref_axis',(1.,0.,0.));
#16955=DIRECTION('',(0.,0.,1.));
#16956=DIRECTION('center_axis',(0.,0.,-1.));
#16957=DIRECTION('ref_axis',(1.,0.,0.));
#16958=DIRECTION('center_axis',(0.,0.,1.));
#16959=DIRECTION('ref_axis',(1.,0.,0.));
#16960=DIRECTION('',(0.,0.,1.));
#16961=DIRECTION('center_axis',(0.,0.,1.));
#16962=DIRECTION('ref_axis',(1.,0.,0.));
#16963=DIRECTION('',(1.,0.,0.));
#16964=DIRECTION('center_axis',(0.,0.,1.));
#16965=DIRECTION('ref_axis',(1.,0.,0.));
#16966=DIRECTION('center_axis',(0.,0.,1.));
#16967=DIRECTION('ref_axis',(1.,0.,0.));
#16968=DIRECTION('',(0.,0.,-1.));
#16969=DIRECTION('center_axis',(0.,0.,1.));
#16970=DIRECTION('ref_axis',(1.,0.,0.));
#16971=DIRECTION('',(0.,0.,1.));
#16972=DIRECTION('center_axis',(0.,0.,-1.));
#16973=DIRECTION('ref_axis',(1.,0.,0.));
#16974=DIRECTION('center_axis',(0.,0.,1.));
#16975=DIRECTION('ref_axis',(1.,0.,0.));
#16976=DIRECTION('',(0.,0.,1.));
#16977=DIRECTION('center_axis',(0.,-1.,0.));
#16978=DIRECTION('ref_axis',(0.,0.,-1.));
#16979=DIRECTION('',(-1.,0.,0.));
#16980=DIRECTION('',(-1.,0.,0.));
#16981=DIRECTION('',(0.,0.,1.));
#16982=DIRECTION('',(1.,0.,0.));
#16983=DIRECTION('',(0.,0.,-1.));
#16984=DIRECTION('',(-1.,0.,0.));
#16985=DIRECTION('center_axis',(0.,1.,0.));
#16986=DIRECTION('ref_axis',(0.,0.,1.));
#16987=DIRECTION('',(1.,0.,0.));
#16988=DIRECTION('',(1.,0.,0.));
#16989=DIRECTION('',(0.,0.,1.));
#16990=DIRECTION('',(1.,0.,0.));
#16991=DIRECTION('',(0.,0.,-1.));
#16992=DIRECTION('',(1.,0.,0.));
#16993=DIRECTION('center_axis',(-1.,0.,0.));
#16994=DIRECTION('ref_axis',(0.,0.,1.));
#16995=DIRECTION('',(0.,-1.,0.));
#16996=DIRECTION('',(0.,0.,1.));
#16997=DIRECTION('',(0.,1.,0.));
#16998=DIRECTION('',(0.,0.,-1.));
#16999=DIRECTION('',(0.,-1.,0.));
#17000=DIRECTION('',(0.,-1.,0.));
#17001=DIRECTION('',(0.,0.,1.));
#17002=DIRECTION('',(0.,-1.,0.));
#17003=DIRECTION('',(0.,0.,-1.));
#17004=DIRECTION('',(0.,-1.,0.));
#17005=DIRECTION('center_axis',(0.,0.,-1.));
#17006=DIRECTION('ref_axis',(0.,1.,0.));
#17007=DIRECTION('',(0.,1.,0.));
#17008=DIRECTION('',(1.,0.,0.));
#17009=DIRECTION('center_axis',(0.,-1.,0.));
#17010=DIRECTION('ref_axis',(0.,0.,-1.));
#17011=DIRECTION('',(0.,0.,-1.));
#17012=DIRECTION('',(1.,0.,0.));
#17013=DIRECTION('center_axis',(0.,0.,1.));
#17014=DIRECTION('ref_axis',(0.,-1.,0.));
#17015=DIRECTION('',(0.,-1.,0.));
#17016=DIRECTION('',(1.,0.,0.));
#17017=DIRECTION('center_axis',(0.,1.,0.));
#17018=DIRECTION('ref_axis',(0.,0.,1.));
#17019=DIRECTION('',(0.,0.,1.));
#17020=DIRECTION('',(1.,0.,0.));
#17021=DIRECTION('center_axis',(0.,0.,-1.));
#17022=DIRECTION('ref_axis',(0.,1.,0.));
#17023=DIRECTION('',(0.,1.,0.));
#17024=DIRECTION('center_axis',(0.,0.,-1.));
#17025=DIRECTION('ref_axis',(0.,1.,0.));
#17026=DIRECTION('',(0.,1.,0.));
#17027=DIRECTION('',(1.,0.,0.));
#17028=DIRECTION('center_axis',(0.,-1.,0.));
#17029=DIRECTION('ref_axis',(0.,0.,-1.));
#17030=DIRECTION('',(0.,0.,-1.));
#17031=DIRECTION('',(1.,0.,0.));
#17032=DIRECTION('center_axis',(0.,0.,-1.));
#17033=DIRECTION('ref_axis',(0.,1.,0.));
#17034=DIRECTION('',(0.,1.,0.));
#17035=DIRECTION('',(1.,0.,0.));
#17036=DIRECTION('center_axis',(0.,1.,0.));
#17037=DIRECTION('ref_axis',(0.,0.,1.));
#17038=DIRECTION('',(0.,0.,1.));
#17039=DIRECTION('',(1.,0.,0.));
#17040=DIRECTION('center_axis',(0.,0.,-1.));
#17041=DIRECTION('ref_axis',(0.,1.,0.));
#17042=DIRECTION('',(0.,1.,0.));
#17043=DIRECTION('center_axis',(1.,0.,0.));
#17044=DIRECTION('ref_axis',(0.,0.,-1.));
#17045=DIRECTION('axis',(0.,0.,1.));
#17046=DIRECTION('refdir',(1.,0.,0.));
#17047=DIRECTION('center_axis',(0.,0.,1.));
#17048=DIRECTION('ref_axis',(0.,-1.,0.));
#17049=DIRECTION('',(0.,-1.,0.));
#17050=DIRECTION('',(1.,0.,0.));
#17051=DIRECTION('',(0.,-1.,0.));
#17052=DIRECTION('',(1.,0.,0.));
#17053=DIRECTION('center_axis',(0.,1.,0.));
#17054=DIRECTION('ref_axis',(0.,0.,1.));
#17055=DIRECTION('',(0.,0.,1.));
#17056=DIRECTION('',(0.,0.,1.));
#17057=DIRECTION('',(1.,0.,0.));
#17058=DIRECTION('center_axis',(0.,0.,-1.));
#17059=DIRECTION('ref_axis',(0.,1.,0.));
#17060=DIRECTION('',(0.,1.,0.));
#17061=DIRECTION('',(0.,1.,0.));
#17062=DIRECTION('',(1.,0.,0.));
#17063=DIRECTION('center_axis',(0.,-1.,0.));
#17064=DIRECTION('ref_axis',(0.,0.,-1.));
#17065=DIRECTION('',(0.,0.,-1.));
#17066=DIRECTION('',(0.,0.,-1.));
#17067=DIRECTION('',(1.,0.,0.));
#17068=DIRECTION('center_axis',(0.,0.,-1.));
#17069=DIRECTION('ref_axis',(0.,1.,0.));
#17070=DIRECTION('',(0.,1.,0.));
#17071=DIRECTION('',(0.,1.,0.));
#17072=DIRECTION('',(1.,0.,0.));
#17073=DIRECTION('center_axis',(0.,1.,0.));
#17074=DIRECTION('ref_axis',(0.,0.,1.));
#17075=DIRECTION('',(0.,0.,1.));
#17076=DIRECTION('',(0.,0.,1.));
#17077=DIRECTION('',(1.,0.,0.));
#17078=DIRECTION('center_axis',(0.,0.,-1.));
#17079=DIRECTION('ref_axis',(0.,1.,0.));
#17080=DIRECTION('',(0.,1.,0.));
#17081=DIRECTION('',(0.,1.,0.));
#17082=DIRECTION('',(1.,0.,0.));
#17083=DIRECTION('center_axis',(0.,-1.,0.));
#17084=DIRECTION('ref_axis',(0.,0.,-1.));
#17085=DIRECTION('',(0.,0.,-1.));
#17086=DIRECTION('',(0.,0.,-1.));
#17087=DIRECTION('center_axis',(1.,0.,0.));
#17088=DIRECTION('ref_axis',(0.,0.,-1.));
#17089=DIRECTION('center_axis',(1.,0.,0.));
#17090=DIRECTION('ref_axis',(0.,0.,-1.));
#17091=DIRECTION('axis',(0.,0.,1.));
#17092=DIRECTION('refdir',(1.,0.,0.));
#17093=DIRECTION('center_axis',(0.,0.,-1.));
#17094=DIRECTION('ref_axis',(0.,-1.,0.));
#17095=DIRECTION('',(0.,1.,0.));
#17096=DIRECTION('',(-1.,0.,0.));
#17097=DIRECTION('',(0.,-1.,0.));
#17098=DIRECTION('',(-1.,0.,0.));
#17099=DIRECTION('center_axis',(0.,1.,0.));
#17100=DIRECTION('ref_axis',(0.,0.,-1.));
#17101=DIRECTION('',(0.,0.,1.));
#17102=DIRECTION('',(0.,0.,-1.));
#17103=DIRECTION('',(-1.,0.,0.));
#17104=DIRECTION('center_axis',(0.,0.,-1.));
#17105=DIRECTION('ref_axis',(0.,-1.,0.));
#17106=DIRECTION('',(0.,1.,0.));
#17107=DIRECTION('',(0.,-1.,0.));
#17108=DIRECTION('',(-1.,0.,0.));
#17109=DIRECTION('center_axis',(0.,-1.,0.));
#17110=DIRECTION('ref_axis',(0.,0.,1.));
#17111=DIRECTION('',(0.,0.,-1.));
#17112=DIRECTION('',(0.,0.,1.));
#17113=DIRECTION('',(-1.,0.,0.));
#17114=DIRECTION('center_axis',(0.,0.,-1.));
#17115=DIRECTION('ref_axis',(0.,-1.,0.));
#17116=DIRECTION('',(0.,1.,0.));
#17117=DIRECTION('',(0.,-1.,0.));
#17118=DIRECTION('',(-1.,0.,0.));
#17119=DIRECTION('center_axis',(0.,1.,0.));
#17120=DIRECTION('ref_axis',(0.,0.,-1.));
#17121=DIRECTION('',(0.,0.,1.));
#17122=DIRECTION('',(0.,0.,-1.));
#17123=DIRECTION('',(-1.,0.,0.));
#17124=DIRECTION('center_axis',(0.,0.,1.));
#17125=DIRECTION('ref_axis',(0.,1.,0.));
#17126=DIRECTION('',(0.,-1.,0.));
#17127=DIRECTION('',(0.,1.,0.));
#17128=DIRECTION('',(-1.,0.,0.));
#17129=DIRECTION('center_axis',(0.,-1.,0.));
#17130=DIRECTION('ref_axis',(0.,0.,1.));
#17131=DIRECTION('',(0.,0.,-1.));
#17132=DIRECTION('',(0.,0.,1.));
#17133=DIRECTION('center_axis',(1.,0.,0.));
#17134=DIRECTION('ref_axis',(0.,0.,-1.));
#17135=DIRECTION('center_axis',(-1.,0.,0.));
#17136=DIRECTION('ref_axis',(0.,0.,1.));
#17137=DIRECTION('',(0.,0.,1.));
#17138=DIRECTION('',(1.,0.,0.));
#17139=DIRECTION('',(0.,0.,1.));
#17140=DIRECTION('',(1.,0.,0.));
#17141=DIRECTION('',(0.,0.,1.));
#17142=DIRECTION('',(1.,0.,0.));
#17143=DIRECTION('axis',(0.,0.,1.));
#17144=DIRECTION('refdir',(1.,0.,0.));
#17145=DIRECTION('center_axis',(0.,1.,0.));
#17146=DIRECTION('ref_axis',(1.,0.,0.));
#17147=DIRECTION('center_axis',(0.,1.,0.));
#17148=DIRECTION('ref_axis',(1.,0.,0.));
#17149=DIRECTION('',(0.707106781186548,-0.707106781186547,-8.65956056235494E-17));
#17150=DIRECTION('center_axis',(0.,-1.,0.));
#17151=DIRECTION('ref_axis',(1.,0.,0.));
#17152=DIRECTION('center_axis',(0.,1.,0.));
#17153=DIRECTION('ref_axis',(1.,0.,0.));
#17154=DIRECTION('',(0.,-1.,0.));
#17155=DIRECTION('center_axis',(0.,-1.,0.));
#17156=DIRECTION('ref_axis',(1.,0.,0.));
#17157=DIRECTION('center_axis',(0.,1.,0.));
#17158=DIRECTION('ref_axis',(1.,0.,0.));
#17159=DIRECTION('center_axis',(0.,1.,0.));
#17160=DIRECTION('ref_axis',(1.,0.,0.));
#17161=DIRECTION('center_axis',(0.,1.,0.));
#17162=DIRECTION('ref_axis',(1.,0.,0.));
#17163=DIRECTION('',(0.,-1.,0.));
#17164=DIRECTION('center_axis',(0.,1.,0.));
#17165=DIRECTION('ref_axis',(1.,0.,0.));
#17166=DIRECTION('center_axis',(0.,1.,0.));
#17167=DIRECTION('ref_axis',(1.,0.,0.));
#17168=DIRECTION('axis',(0.,0.,1.));
#17169=DIRECTION('refdir',(1.,0.,0.));
#17170=DIRECTION('center_axis',(0.866025403784439,0.,-0.5));
#17171=DIRECTION('ref_axis',(0.5,0.,0.866025403784439));
#17172=DIRECTION('',(-0.5,0.,-0.866025403784439));
#17173=DIRECTION('',(0.,-1.,0.));
#17174=DIRECTION('',(0.5,0.,0.866025403784439));
#17175=DIRECTION('',(0.,-1.,0.));
#17176=DIRECTION('center_axis',(1.20185167898973E-16,0.,-1.));
#17177=DIRECTION('ref_axis',(1.,0.,1.20185167898973E-16));
#17178=DIRECTION('',(-1.,0.,-1.20185167898973E-16));
#17179=DIRECTION('',(0.,-1.,0.));
#17180=DIRECTION('',(1.,0.,1.20185167898973E-16));
#17181=DIRECTION('center_axis',(-0.866025403784439,0.,-0.5));
#17182=DIRECTION('ref_axis',(0.5,0.,-0.866025403784439));
#17183=DIRECTION('',(-0.5,0.,0.866025403784439));
#17184=DIRECTION('',(0.,-1.,0.));
#17185=DIRECTION('',(0.5,0.,-0.866025403784439));
#17186=DIRECTION('center_axis',(-0.866025403784439,0.,0.5));
#17187=DIRECTION('ref_axis',(-0.5,0.,-0.866025403784439));
#17188=DIRECTION('',(0.5,0.,0.866025403784439));
#17189=DIRECTION('',(0.,-1.,0.));
#17190=DIRECTION('',(-0.5,0.,-0.866025403784439));
#17191=DIRECTION('center_axis',(-2.40370335797945E-16,0.,1.));
#17192=DIRECTION('ref_axis',(-1.,0.,-2.40370335797945E-16));
#17193=DIRECTION('',(1.,0.,2.40370335797945E-16));
#17194=DIRECTION('',(0.,-1.,0.));
#17195=DIRECTION('',(-1.,0.,-2.40370335797945E-16));
#17196=DIRECTION('center_axis',(0.866025403784439,0.,0.5));
#17197=DIRECTION('ref_axis',(-0.5,0.,0.866025403784439));
#17198=DIRECTION('',(0.5,0.,-0.866025403784439));
#17199=DIRECTION('',(-0.5,0.,0.866025403784439));
#17200=DIRECTION('center_axis',(0.,1.,0.));
#17201=DIRECTION('ref_axis',(1.,0.,0.));
#17202=DIRECTION('center_axis',(0.,-1.,0.));
#17203=DIRECTION('ref_axis',(0.,0.,-1.));
#17204=DIRECTION('center_axis',(0.,1.,0.));
#17205=DIRECTION('ref_axis',(1.,0.,0.));
#17206=DIRECTION('center_axis',(0.,1.,0.));
#17207=DIRECTION('ref_axis',(1.,0.,0.));
#17208=DIRECTION('center_axis',(0.,1.,0.));
#17209=DIRECTION('ref_axis',(1.,0.,0.));
#17210=DIRECTION('center_axis',(0.,1.,0.));
#17211=DIRECTION('ref_axis',(1.,0.,0.));
#17212=DIRECTION('',(0.,-1.,0.));
#17213=DIRECTION('center_axis',(0.,1.,0.));
#17214=DIRECTION('ref_axis',(1.,0.,0.));
#17215=DIRECTION('center_axis',(0.,1.,0.));
#17216=DIRECTION('ref_axis',(1.,0.,0.));
#17217=DIRECTION('center_axis',(0.,1.,0.));
#17218=DIRECTION('ref_axis',(0.,0.,1.));
#17219=DIRECTION('center_axis',(0.,-1.,0.));
#17220=DIRECTION('ref_axis',(1.,0.,0.));
#17221=DIRECTION('center_axis',(0.,-1.,0.));
#17222=DIRECTION('ref_axis',(1.,0.,0.));
#17223=DIRECTION('center_axis',(0.,-1.,0.));
#17224=DIRECTION('ref_axis',(1.,0.,0.));
#17225=DIRECTION('',(0.707106781186548,0.707106781186547,8.65956056235493E-17));
#17226=DIRECTION('center_axis',(0.,-1.,0.));
#17227=DIRECTION('ref_axis',(1.,0.,0.));
#17228=DIRECTION('center_axis',(0.,-1.,0.));
#17229=DIRECTION('ref_axis',(1.,0.,0.));
#17230=DIRECTION('',(0.,1.,0.));
#17231=DIRECTION('center_axis',(0.,1.,0.));
#17232=DIRECTION('ref_axis',(1.,0.,0.));
#17233=DIRECTION('center_axis',(0.,-1.,0.));
#17234=DIRECTION('ref_axis',(1.,0.,0.));
#17235=DIRECTION('',(-0.707106781186547,0.707106781186548,-8.65956056235493E-17));
#17236=DIRECTION('center_axis',(0.,-1.,0.));
#17237=DIRECTION('ref_axis',(0.,0.,-1.));
#17238=DIRECTION('center_axis',(0.,-1.,0.));
#17239=DIRECTION('ref_axis',(1.,0.,0.));
#17240=DIRECTION('center_axis',(0.,1.,0.));
#17241=DIRECTION('ref_axis',(1.,0.,0.));
#17242=DIRECTION('center_axis',(0.,1.,0.));
#17243=DIRECTION('ref_axis',(1.,0.,0.));
#17244=DIRECTION('',(-0.447213595499958,0.894427190999916,-5.47678698264203E-17));
#17245=DIRECTION('center_axis',(0.,-1.,0.));
#17246=DIRECTION('ref_axis',(1.,0.,0.));
#17247=DIRECTION('',(0.,1.,0.));
#17248=DIRECTION('axis',(0.,0.,1.));
#17249=DIRECTION('refdir',(1.,0.,0.));
#17250=DIRECTION('center_axis',(1.,0.,0.));
#17251=DIRECTION('ref_axis',(0.,0.207879895528894,-0.978154358490978));
#17252=DIRECTION('',(-1.,0.,0.));
#17253=DIRECTION('center_axis',(1.,0.,0.));
#17254=DIRECTION('ref_axis',(0.,0.,-1.));
#17255=DIRECTION('center_axis',(1.,0.,0.));
#17256=DIRECTION('ref_axis',(0.,0.,-1.));
#17257=DIRECTION('',(-1.,0.,0.));
#17258=DIRECTION('center_axis',(1.,0.,0.));
#17259=DIRECTION('ref_axis',(0.,0.,-1.));
#17260=DIRECTION('',(-1.,0.,0.));
#17261=DIRECTION('center_axis',(1.,0.,0.));
#17262=DIRECTION('ref_axis',(0.,0.,-1.));
#17263=DIRECTION('',(-1.,0.,0.));
#17264=DIRECTION('center_axis',(1.,0.,0.));
#17265=DIRECTION('ref_axis',(0.,0.,-1.));
#17266=DIRECTION('',(-1.,0.,0.));
#17267=DIRECTION('center_axis',(1.,0.,0.));
#17268=DIRECTION('ref_axis',(0.,0.,-1.));
#17269=DIRECTION('',(-1.,0.,0.));
#17270=DIRECTION('center_axis',(1.,0.,0.));
#17271=DIRECTION('ref_axis',(0.,0.,-1.));
#17272=DIRECTION('',(-1.,0.,0.));
#17273=DIRECTION('center_axis',(1.,0.,0.));
#17274=DIRECTION('ref_axis',(0.,0.,-1.));
#17275=DIRECTION('',(-1.,0.,0.));
#17276=DIRECTION('center_axis',(1.,0.,0.));
#17277=DIRECTION('ref_axis',(0.,0.,-1.));
#17278=DIRECTION('',(-1.,0.,0.));
#17279=DIRECTION('center_axis',(1.,0.,0.));
#17280=DIRECTION('ref_axis',(0.,0.,-1.));
#17281=DIRECTION('center_axis',(1.,0.,0.));
#17282=DIRECTION('ref_axis',(0.,2.68771689099506E-14,-1.));
#17283=DIRECTION('',(1.,3.30650148539799E-30,-1.22464679914735E-16));
#17284=DIRECTION('center_axis',(-1.,0.,0.));
#17285=DIRECTION('ref_axis',(0.,2.68771689099506E-14,-1.));
#17286=DIRECTION('center_axis',(1.,0.,0.));
#17287=DIRECTION('ref_axis',(0.,2.68771689099506E-14,-1.));
#17288=DIRECTION('',(1.,3.30650148539799E-30,-1.22464679914735E-16));
#17289=DIRECTION('center_axis',(1.,0.,0.));
#17290=DIRECTION('ref_axis',(0.,2.68771689099506E-14,-1.));
#17291=DIRECTION('',(1.,3.30650148539799E-30,-1.22464679914735E-16));
#17292=DIRECTION('center_axis',(1.,0.,0.));
#17293=DIRECTION('ref_axis',(0.,2.68771689099506E-14,-1.));
#17294=DIRECTION('',(1.,3.30650148539799E-30,-1.22464679914735E-16));
#17295=DIRECTION('center_axis',(1.,0.,0.));
#17296=DIRECTION('ref_axis',(0.,2.68771689099506E-14,-1.));
#17297=DIRECTION('',(1.,3.30650148539799E-30,-1.22464679914735E-16));
#17298=DIRECTION('center_axis',(1.,0.,0.));
#17299=DIRECTION('ref_axis',(0.,2.68771689099506E-14,-1.));
#17300=DIRECTION('',(1.,3.30650148539799E-30,-1.22464679914735E-16));
#17301=DIRECTION('center_axis',(1.,0.,0.));
#17302=DIRECTION('ref_axis',(0.,2.68771689099506E-14,-1.));
#17303=DIRECTION('',(1.,3.30650148539799E-30,-1.22464679914735E-16));
#17304=DIRECTION('center_axis',(1.,0.,0.));
#17305=DIRECTION('ref_axis',(0.,2.68771689099506E-14,-1.));
#17306=DIRECTION('',(1.,3.30650148539799E-30,-1.22464679914735E-16));
#17307=DIRECTION('center_axis',(1.,0.,0.));
#17308=DIRECTION('ref_axis',(0.,2.68771689099506E-14,-1.));
#17309=DIRECTION('',(1.,3.30650148539799E-30,-1.22464679914735E-16));
#17310=DIRECTION('center_axis',(1.,0.,0.));
#17311=DIRECTION('ref_axis',(0.,2.68771689099506E-14,-1.));
#17312=DIRECTION('center_axis',(1.,0.,0.));
#17313=DIRECTION('ref_axis',(0.,2.68771689099506E-14,-1.));
#17314=DIRECTION('center_axis',(1.,0.,0.));
#17315=DIRECTION('ref_axis',(0.,0.,-1.));
#17316=DIRECTION('',(0.,1.,0.));
#17317=DIRECTION('center_axis',(1.,0.,0.));
#17318=DIRECTION('ref_axis',(0.,0.,-1.));
#17319=DIRECTION('center_axis',(1.,0.,0.));
#17320=DIRECTION('ref_axis',(0.,0.,-1.));
#17321=DIRECTION('center_axis',(-1.,0.,0.));
#17322=DIRECTION('ref_axis',(0.,0.,-1.));
#17323=DIRECTION('center_axis',(-1.,0.,0.));
#17324=DIRECTION('ref_axis',(0.,0.,-1.));
#17325=DIRECTION('center_axis',(-1.,0.,0.));
#17326=DIRECTION('ref_axis',(0.,0.,-1.));
#17327=DIRECTION('center_axis',(1.,0.,0.));
#17328=DIRECTION('ref_axis',(0.,0.,-1.));
#17329=DIRECTION('center_axis',(1.,0.,0.));
#17330=DIRECTION('ref_axis',(0.,0.,-1.));
#17331=DIRECTION('',(1.,0.,0.));
#17332=DIRECTION('center_axis',(1.,0.,0.));
#17333=DIRECTION('ref_axis',(0.,0.,-1.));
#17334=DIRECTION('center_axis',(1.,0.,0.));
#17335=DIRECTION('ref_axis',(0.,0.,-1.));
#17336=DIRECTION('',(1.,0.,0.));
#17337=DIRECTION('center_axis',(1.,0.,0.));
#17338=DIRECTION('ref_axis',(0.,0.,-1.));
#17339=DIRECTION('center_axis',(1.,0.,0.));
#17340=DIRECTION('ref_axis',(0.,0.,-1.));
#17341=DIRECTION('',(1.,0.,0.));
#17342=DIRECTION('center_axis',(0.,0.,1.));
#17343=DIRECTION('ref_axis',(0.,-1.,0.));
#17344=DIRECTION('',(0.,-1.,0.));
#17345=DIRECTION('',(-1.,0.,0.));
#17346=DIRECTION('',(1.,0.,0.));
#17347=DIRECTION('center_axis',(1.,0.,0.));
#17348=DIRECTION('ref_axis',(0.,0.,-1.));
#17349=DIRECTION('center_axis',(1.,0.,0.));
#17350=DIRECTION('ref_axis',(0.,0.,-1.));
#17351=DIRECTION('center_axis',(1.,0.,0.));
#17352=DIRECTION('ref_axis',(0.,0.,-1.));
#17353=DIRECTION('center_axis',(1.,0.,0.));
#17354=DIRECTION('ref_axis',(0.,-1.22464679914735E-16,1.));
#17355=DIRECTION('center_axis',(1.,0.,0.));
#17356=DIRECTION('ref_axis',(0.,0.,-1.));
#17357=DIRECTION('center_axis',(1.,0.,0.));
#17358=DIRECTION('ref_axis',(0.,0.,-1.));
#17359=DIRECTION('',(-1.,0.,0.));
#17360=DIRECTION('center_axis',(1.,0.,0.));
#17361=DIRECTION('ref_axis',(0.,0.,-1.));
#17362=DIRECTION('center_axis',(1.,0.,0.));
#17363=DIRECTION('ref_axis',(0.,0.,-1.));
#17364=DIRECTION('axis',(0.,0.,1.));
#17365=DIRECTION('refdir',(1.,0.,0.));
#17366=DIRECTION('center_axis',(0.,1.,0.));
#17367=DIRECTION('ref_axis',(0.,0.,1.));
#17368=DIRECTION('center_axis',(0.,-1.,0.));
#17369=DIRECTION('ref_axis',(1.,0.,0.));
#17370=DIRECTION('center_axis',(0.,-1.,0.));
#17371=DIRECTION('ref_axis',(1.,0.,0.));
#17372=DIRECTION('center_axis',(0.,-1.,0.));
#17373=DIRECTION('ref_axis',(1.,0.,0.));
#17374=DIRECTION('',(0.707106781186547,0.707106781186548,8.65956056235493E-17));
#17375=DIRECTION('center_axis',(0.,-1.,0.));
#17376=DIRECTION('ref_axis',(1.,0.,0.));
#17377=DIRECTION('center_axis',(0.,-1.,0.));
#17378=DIRECTION('ref_axis',(1.,0.,0.));
#17379=DIRECTION('',(0.,1.,0.));
#17380=DIRECTION('center_axis',(0.,1.,0.));
#17381=DIRECTION('ref_axis',(1.,0.,0.));
#17382=DIRECTION('center_axis',(0.,-1.,0.));
#17383=DIRECTION('ref_axis',(1.,0.,0.));
#17384=DIRECTION('',(-0.707106781186547,0.707106781186548,-8.65956056235493E-17));
#17385=DIRECTION('center_axis',(0.,-1.,0.));
#17386=DIRECTION('ref_axis',(0.,0.,-1.));
#17387=DIRECTION('center_axis',(0.,-1.,0.));
#17388=DIRECTION('ref_axis',(1.,0.,0.));
#17389=DIRECTION('center_axis',(0.,1.,0.));
#17390=DIRECTION('ref_axis',(1.,0.,0.));
#17391=DIRECTION('center_axis',(0.,1.,0.));
#17392=DIRECTION('ref_axis',(1.,0.,0.));
#17393=DIRECTION('',(-0.447213595499958,0.894427190999916,-5.47678698264203E-17));
#17394=DIRECTION('center_axis',(0.,-1.,0.));
#17395=DIRECTION('ref_axis',(1.,0.,0.));
#17396=DIRECTION('center_axis',(0.,1.,0.));
#17397=DIRECTION('ref_axis',(1.,0.,0.));
#17398=DIRECTION('',(0.,1.,0.));
#17399=DIRECTION('center_axis',(0.,1.,0.));
#17400=DIRECTION('ref_axis',(1.,0.,0.));
#17401=DIRECTION('center_axis',(0.,-1.,0.));
#17402=DIRECTION('ref_axis',(1.,0.,0.));
#17403=DIRECTION('',(-0.707106781186547,0.707106781186548,-8.65956056235493E-17));
#17404=DIRECTION('center_axis',(0.,-1.,0.));
#17405=DIRECTION('ref_axis',(0.,0.,-1.));
#17406=DIRECTION('center_axis',(0.866025403784439,0.,-0.5));
#17407=DIRECTION('ref_axis',(0.5,0.,0.866025403784439));
#17408=DIRECTION('',(-0.5,0.,-0.866025403784439));
#17409=DIRECTION('',(0.,-1.,0.));
#17410=DIRECTION('',(0.5,0.,0.866025403784439));
#17411=DIRECTION('',(0.,-1.,0.));
#17412=DIRECTION('center_axis',(1.60246890531964E-16,0.,-1.));
#17413=DIRECTION('ref_axis',(1.,0.,1.60246890531964E-16));
#17414=DIRECTION('',(-1.,0.,-1.60246890531964E-16));
#17415=DIRECTION('',(0.,-1.,0.));
#17416=DIRECTION('',(1.,0.,1.60246890531964E-16));
#17417=DIRECTION('center_axis',(-0.866025403784439,0.,-0.5));
#17418=DIRECTION('ref_axis',(0.5,0.,-0.866025403784439));
#17419=DIRECTION('',(-0.5,0.,0.866025403784439));
#17420=DIRECTION('',(0.,-1.,0.));
#17421=DIRECTION('',(0.5,0.,-0.866025403784439));
#17422=DIRECTION('center_axis',(-0.866025403784439,0.,0.5));
#17423=DIRECTION('ref_axis',(-0.5,0.,-0.866025403784439));
#17424=DIRECTION('',(0.5,0.,0.866025403784439));
#17425=DIRECTION('',(0.,-1.,0.));
#17426=DIRECTION('',(-0.5,0.,-0.866025403784439));
#17427=DIRECTION('center_axis',(-1.60246890531964E-16,0.,1.));
#17428=DIRECTION('ref_axis',(-1.,0.,-1.60246890531964E-16));
#17429=DIRECTION('',(1.,0.,1.60246890531964E-16));
#17430=DIRECTION('',(0.,-1.,0.));
#17431=DIRECTION('',(-1.,0.,-1.60246890531964E-16));
#17432=DIRECTION('center_axis',(0.866025403784439,0.,0.5));
#17433=DIRECTION('ref_axis',(-0.5,0.,0.866025403784439));
#17434=DIRECTION('',(0.5,0.,-0.866025403784439));
#17435=DIRECTION('',(-0.5,0.,0.866025403784439));
#17436=DIRECTION('center_axis',(0.,1.,0.));
#17437=DIRECTION('ref_axis',(1.,0.,0.));
#17438=DIRECTION('center_axis',(0.,-1.,0.));
#17439=DIRECTION('ref_axis',(0.,0.,-1.));
#17440=DIRECTION('axis',(0.,0.,1.));
#17441=DIRECTION('refdir',(1.,0.,0.));
#17442=DIRECTION('center_axis',(0.,1.,0.));
#17443=DIRECTION('ref_axis',(0.,0.,1.));
#17444=DIRECTION('center_axis',(0.,-1.,0.));
#17445=DIRECTION('ref_axis',(1.,0.,0.));
#17446=DIRECTION('center_axis',(0.,-1.,0.));
#17447=DIRECTION('ref_axis',(1.,0.,0.));
#17448=DIRECTION('center_axis',(0.,-1.,0.));
#17449=DIRECTION('ref_axis',(1.,0.,0.));
#17450=DIRECTION('',(0.707106781186548,0.707106781186547,8.65956056235493E-17));
#17451=DIRECTION('center_axis',(0.,-1.,0.));
#17452=DIRECTION('ref_axis',(1.,0.,0.));
#17453=DIRECTION('center_axis',(0.,-1.,0.));
#17454=DIRECTION('ref_axis',(1.,0.,0.));
#17455=DIRECTION('',(0.,1.,0.));
#17456=DIRECTION('center_axis',(0.,1.,0.));
#17457=DIRECTION('ref_axis',(1.,0.,0.));
#17458=DIRECTION('center_axis',(0.,-1.,0.));
#17459=DIRECTION('ref_axis',(1.,0.,0.));
#17460=DIRECTION('',(-0.707106781186547,0.707106781186548,-8.65956056235493E-17));
#17461=DIRECTION('center_axis',(0.,-1.,0.));
#17462=DIRECTION('ref_axis',(0.,0.,-1.));
#17463=DIRECTION('center_axis',(0.,-1.,0.));
#17464=DIRECTION('ref_axis',(1.,0.,0.));
#17465=DIRECTION('center_axis',(0.,1.,0.));
#17466=DIRECTION('ref_axis',(1.,0.,0.));
#17467=DIRECTION('center_axis',(0.,1.,0.));
#17468=DIRECTION('ref_axis',(1.,0.,0.));
#17469=DIRECTION('',(-0.447213595499958,0.894427190999916,-5.47678698264203E-17));
#17470=DIRECTION('center_axis',(0.,-1.,0.));
#17471=DIRECTION('ref_axis',(1.,0.,0.));
#17472=DIRECTION('center_axis',(0.,1.,0.));
#17473=DIRECTION('ref_axis',(1.,0.,0.));
#17474=DIRECTION('',(0.,1.,0.));
#17475=DIRECTION('center_axis',(0.,1.,0.));
#17476=DIRECTION('ref_axis',(1.,0.,0.));
#17477=DIRECTION('center_axis',(0.,-1.,0.));
#17478=DIRECTION('ref_axis',(1.,0.,0.));
#17479=DIRECTION('',(-0.707106781186547,0.707106781186548,-8.65956056235493E-17));
#17480=DIRECTION('center_axis',(0.,-1.,0.));
#17481=DIRECTION('ref_axis',(0.,0.,-1.));
#17482=DIRECTION('center_axis',(0.866025403784439,0.,-0.5));
#17483=DIRECTION('ref_axis',(0.5,0.,0.866025403784439));
#17484=DIRECTION('',(-0.5,0.,-0.866025403784439));
#17485=DIRECTION('',(0.,-1.,0.));
#17486=DIRECTION('',(0.5,0.,0.866025403784439));
#17487=DIRECTION('',(0.,-1.,0.));
#17488=DIRECTION('center_axis',(1.20185167898973E-16,0.,-1.));
#17489=DIRECTION('ref_axis',(1.,0.,1.20185167898973E-16));
#17490=DIRECTION('',(-1.,0.,-1.20185167898973E-16));
#17491=DIRECTION('',(0.,-1.,0.));
#17492=DIRECTION('',(1.,0.,1.20185167898973E-16));
#17493=DIRECTION('center_axis',(-0.866025403784439,0.,-0.5));
#17494=DIRECTION('ref_axis',(0.5,0.,-0.866025403784439));
#17495=DIRECTION('',(-0.5,0.,0.866025403784439));
#17496=DIRECTION('',(0.,-1.,0.));
#17497=DIRECTION('',(0.5,0.,-0.866025403784439));
#17498=DIRECTION('center_axis',(-0.866025403784439,0.,0.5));
#17499=DIRECTION('ref_axis',(-0.5,0.,-0.866025403784439));
#17500=DIRECTION('',(0.5,0.,0.866025403784439));
#17501=DIRECTION('',(0.,-1.,0.));
#17502=DIRECTION('',(-0.5,0.,-0.866025403784439));
#17503=DIRECTION('center_axis',(-2.40370335797945E-16,0.,1.));
#17504=DIRECTION('ref_axis',(-1.,0.,-2.40370335797945E-16));
#17505=DIRECTION('',(1.,0.,2.40370335797945E-16));
#17506=DIRECTION('',(0.,-1.,0.));
#17507=DIRECTION('',(-1.,0.,-2.40370335797945E-16));
#17508=DIRECTION('center_axis',(0.866025403784439,0.,0.5));
#17509=DIRECTION('ref_axis',(-0.5,0.,0.866025403784439));
#17510=DIRECTION('',(0.5,0.,-0.866025403784439));
#17511=DIRECTION('',(-0.5,0.,0.866025403784439));
#17512=DIRECTION('center_axis',(0.,1.,0.));
#17513=DIRECTION('ref_axis',(1.,0.,0.));
#17514=DIRECTION('center_axis',(0.,-1.,0.));
#17515=DIRECTION('ref_axis',(0.,0.,-1.));
#17516=DIRECTION('',(0.,0.,1.));
#17517=DIRECTION('',(1.,0.,0.));
#17518=DIRECTION('',(0.,0.,1.));
#17519=DIRECTION('',(1.,0.,0.));
#17520=DIRECTION('',(0.,0.,1.));
#17521=DIRECTION('',(1.,0.,0.));
#17522=DIRECTION('',(0.,0.,1.));
#17523=DIRECTION('',(1.,0.,0.));
#17524=DIRECTION('',(0.,-1.,2.22044604925031E-16));
#17525=DIRECTION('',(1.,0.,0.));
#17526=DIRECTION('',(0.,-1.,2.22044604925031E-16));
#17527=DIRECTION('',(1.,0.,0.));
#17528=DIRECTION('',(0.,-1.,2.22044604925031E-16));
#17529=DIRECTION('',(1.,0.,0.));
#17530=DIRECTION('',(0.,-1.,2.22044604925031E-16));
#17531=DIRECTION('',(1.,0.,0.));
#17532=DIRECTION('',(0.,-1.,2.22044604925031E-16));
#17533=DIRECTION('',(1.,0.,0.));
#17534=DIRECTION('',(0.,-1.,2.22044604925031E-16));
#17535=DIRECTION('',(1.,0.,0.));
#17536=DIRECTION('',(0.,-1.,2.22044604925031E-16));
#17537=DIRECTION('',(1.,0.,0.));
#17538=DIRECTION('',(0.,-1.,2.22044604925031E-16));
#17539=DIRECTION('',(1.,0.,0.));
#17540=DIRECTION('',(0.,0.,1.));
#17541=DIRECTION('',(1.,0.,0.));
#17542=DIRECTION('',(0.,0.,1.));
#17543=DIRECTION('',(2.22044604925031E-16,-1.,0.));
#17544=DIRECTION('',(0.,0.,1.));
#17545=DIRECTION('',(2.22044604925031E-16,-1.,0.));
#17546=DIRECTION('',(0.,0.,1.));
#17547=DIRECTION('',(2.22044604925031E-16,-1.,0.));
#17548=DIRECTION('',(0.,-1.,2.22044604925031E-16));
#17549=DIRECTION('',(1.,0.,0.));
#17550=DIRECTION('',(0.,-1.,2.22044604925031E-16));
#17551=DIRECTION('',(1.,0.,0.));
#17552=DIRECTION('',(0.,-1.,2.22044604925031E-16));
#17553=DIRECTION('',(1.,0.,0.));
#17554=DIRECTION('',(0.,-1.,2.22044604925031E-16));
#17555=DIRECTION('',(1.,0.,0.));
#17556=DIRECTION('axis',(0.,0.,1.));
#17557=DIRECTION('refdir',(1.,0.,0.));
#17558=DIRECTION('axis',(0.,0.,1.));
#17559=DIRECTION('refdir',(1.,0.,0.));
#17560=DIRECTION('center_axis',(1.,0.,0.));
#17561=DIRECTION('ref_axis',(0.,0.975560628713931,0.219730425074181));
#17562=DIRECTION('',(-1.,0.,0.));
#17563=DIRECTION('center_axis',(-1.,0.,0.));
#17564=DIRECTION('ref_axis',(0.,0.,-1.));
#17565=DIRECTION('center_axis',(1.,0.,0.));
#17566=DIRECTION('ref_axis',(0.,0.,-1.));
#17567=DIRECTION('',(-1.,0.,0.));
#17568=DIRECTION('center_axis',(1.,0.,0.));
#17569=DIRECTION('ref_axis',(0.,0.,-1.));
#17570=DIRECTION('',(-1.,0.,0.));
#17571=DIRECTION('center_axis',(1.,0.,0.));
#17572=DIRECTION('ref_axis',(0.,0.,-1.));
#17573=DIRECTION('',(-1.,0.,0.));
#17574=DIRECTION('center_axis',(1.,0.,0.));
#17575=DIRECTION('ref_axis',(0.,0.,-1.));
#17576=DIRECTION('',(-1.,0.,0.));
#17577=DIRECTION('center_axis',(1.,0.,0.));
#17578=DIRECTION('ref_axis',(0.,0.,-1.));
#17579=DIRECTION('',(-1.,0.,0.));
#17580=DIRECTION('center_axis',(1.,0.,0.));
#17581=DIRECTION('ref_axis',(0.,0.,-1.));
#17582=DIRECTION('',(-1.,0.,0.));
#17583=DIRECTION('center_axis',(1.,0.,0.));
#17584=DIRECTION('ref_axis',(0.,0.,-1.));
#17585=DIRECTION('',(-1.,0.,0.));
#17586=DIRECTION('center_axis',(1.,0.,0.));
#17587=DIRECTION('ref_axis',(0.,0.,-1.));
#17588=DIRECTION('',(-1.,0.,0.));
#17589=DIRECTION('center_axis',(1.,0.,0.));
#17590=DIRECTION('ref_axis',(0.,0.,-1.));
#17591=DIRECTION('',(-1.,0.,0.));
#17592=DIRECTION('center_axis',(1.,0.,0.));
#17593=DIRECTION('ref_axis',(0.,0.,-1.));
#17594=DIRECTION('',(-1.,0.,0.));
#17595=DIRECTION('center_axis',(1.,0.,0.));
#17596=DIRECTION('ref_axis',(0.,0.,-1.));
#17597=DIRECTION('',(-1.,0.,0.));
#17598=DIRECTION('center_axis',(1.,0.,0.));
#17599=DIRECTION('ref_axis',(0.,0.,-1.));
#17600=DIRECTION('',(-1.,0.,0.));
#17601=DIRECTION('center_axis',(1.,0.,0.));
#17602=DIRECTION('ref_axis',(0.,0.,-1.));
#17603=DIRECTION('',(-1.,0.,0.));
#17604=DIRECTION('center_axis',(1.,0.,0.));
#17605=DIRECTION('ref_axis',(0.,0.,-1.));
#17606=DIRECTION('',(-1.,0.,0.));
#17607=DIRECTION('center_axis',(1.,0.,0.));
#17608=DIRECTION('ref_axis',(0.,0.,-1.));
#17609=DIRECTION('',(-1.,0.,0.));
#17610=DIRECTION('center_axis',(1.,0.,0.));
#17611=DIRECTION('ref_axis',(0.,0.,-1.));
#17612=DIRECTION('',(-1.,0.,0.));
#17613=DIRECTION('center_axis',(1.,0.,0.));
#17614=DIRECTION('ref_axis',(0.,0.,-1.));
#17615=DIRECTION('',(-1.,0.,0.));
#17616=DIRECTION('center_axis',(1.,0.,0.));
#17617=DIRECTION('ref_axis',(0.,0.,-1.));
#17618=DIRECTION('',(-1.,0.,0.));
#17619=DIRECTION('center_axis',(1.,0.,0.));
#17620=DIRECTION('ref_axis',(0.,0.,-1.));
#17621=DIRECTION('',(-1.,0.,0.));
#17622=DIRECTION('center_axis',(1.,0.,0.));
#17623=DIRECTION('ref_axis',(0.,0.,-1.));
#17624=DIRECTION('',(-1.,0.,0.));
#17625=DIRECTION('center_axis',(1.,0.,0.));
#17626=DIRECTION('ref_axis',(0.,0.,-1.));
#17627=DIRECTION('',(-1.,0.,0.));
#17628=DIRECTION('center_axis',(1.,0.,0.));
#17629=DIRECTION('ref_axis',(0.,0.,-1.));
#17630=DIRECTION('',(-1.,0.,0.));
#17631=DIRECTION('center_axis',(1.,0.,0.));
#17632=DIRECTION('ref_axis',(0.,0.,-1.));
#17633=DIRECTION('',(-1.,0.,0.));
#17634=DIRECTION('center_axis',(1.,0.,0.));
#17635=DIRECTION('ref_axis',(0.,0.,-1.));
#17636=DIRECTION('',(-1.,0.,0.));
#17637=DIRECTION('center_axis',(1.,0.,0.));
#17638=DIRECTION('ref_axis',(0.,0.,-1.));
#17639=DIRECTION('',(-1.,0.,0.));
#17640=DIRECTION('center_axis',(1.,0.,0.));
#17641=DIRECTION('ref_axis',(0.,0.,-1.));
#17642=DIRECTION('',(-1.,0.,0.));
#17643=DIRECTION('center_axis',(1.,0.,0.));
#17644=DIRECTION('ref_axis',(0.,0.,-1.));
#17645=DIRECTION('',(-1.,0.,0.));
#17646=DIRECTION('center_axis',(1.,0.,0.));
#17647=DIRECTION('ref_axis',(0.,0.,-1.));
#17648=DIRECTION('',(-1.,0.,0.));
#17649=DIRECTION('center_axis',(1.,0.,0.));
#17650=DIRECTION('ref_axis',(0.,0.,-1.));
#17651=DIRECTION('',(-1.,0.,0.));
#17652=DIRECTION('center_axis',(1.,0.,0.));
#17653=DIRECTION('ref_axis',(0.,0.,-1.));
#17654=DIRECTION('',(-1.,0.,0.));
#17655=DIRECTION('center_axis',(1.,0.,0.));
#17656=DIRECTION('ref_axis',(0.,0.,-1.));
#17657=DIRECTION('',(-1.,0.,0.));
#17658=DIRECTION('center_axis',(1.,0.,0.));
#17659=DIRECTION('ref_axis',(0.,0.,-1.));
#17660=DIRECTION('',(-1.,0.,0.));
#17661=DIRECTION('center_axis',(1.,0.,0.));
#17662=DIRECTION('ref_axis',(0.,0.,-1.));
#17663=DIRECTION('',(-1.,0.,0.));
#17664=DIRECTION('center_axis',(1.,0.,0.));
#17665=DIRECTION('ref_axis',(0.,0.,-1.));
#17666=DIRECTION('',(-1.,0.,0.));
#17667=DIRECTION('center_axis',(1.,0.,0.));
#17668=DIRECTION('ref_axis',(0.,0.,-1.));
#17669=DIRECTION('',(-1.,0.,0.));
#17670=DIRECTION('center_axis',(1.,0.,0.));
#17671=DIRECTION('ref_axis',(0.,0.,-1.));
#17672=DIRECTION('',(-1.,0.,0.));
#17673=DIRECTION('center_axis',(1.,0.,0.));
#17674=DIRECTION('ref_axis',(0.,0.,-1.));
#17675=DIRECTION('',(-1.,0.,0.));
#17676=DIRECTION('center_axis',(1.,0.,0.));
#17677=DIRECTION('ref_axis',(0.,0.,-1.));
#17678=DIRECTION('',(-1.,0.,0.));
#17679=DIRECTION('center_axis',(1.,0.,0.));
#17680=DIRECTION('ref_axis',(0.,0.,-1.));
#17681=DIRECTION('',(-1.,0.,0.));
#17682=DIRECTION('center_axis',(1.,0.,0.));
#17683=DIRECTION('ref_axis',(0.,0.,-1.));
#17684=DIRECTION('',(-1.,0.,0.));
#17685=DIRECTION('center_axis',(1.,0.,0.));
#17686=DIRECTION('ref_axis',(0.,0.,-1.));
#17687=DIRECTION('',(-1.,0.,0.));
#17688=DIRECTION('center_axis',(1.,0.,0.));
#17689=DIRECTION('ref_axis',(0.,0.,-1.));
#17690=DIRECTION('',(-1.,0.,0.));
#17691=DIRECTION('center_axis',(1.,0.,0.));
#17692=DIRECTION('ref_axis',(0.,0.,-1.));
#17693=DIRECTION('',(-1.,0.,0.));
#17694=DIRECTION('center_axis',(1.,0.,0.));
#17695=DIRECTION('ref_axis',(0.,0.,-1.));
#17696=DIRECTION('',(-1.,0.,0.));
#17697=DIRECTION('center_axis',(1.,0.,0.));
#17698=DIRECTION('ref_axis',(0.,0.,-1.));
#17699=DIRECTION('',(-1.,0.,0.));
#17700=DIRECTION('center_axis',(1.,0.,0.));
#17701=DIRECTION('ref_axis',(0.,0.,-1.));
#17702=DIRECTION('',(-1.,0.,0.));
#17703=DIRECTION('center_axis',(1.,0.,0.));
#17704=DIRECTION('ref_axis',(0.,0.,-1.));
#17705=DIRECTION('',(-1.,0.,0.));
#17706=DIRECTION('center_axis',(1.,0.,0.));
#17707=DIRECTION('ref_axis',(0.,0.,-1.));
#17708=DIRECTION('',(-1.,0.,0.));
#17709=DIRECTION('center_axis',(1.,0.,0.));
#17710=DIRECTION('ref_axis',(0.,0.,-1.));
#17711=DIRECTION('',(-1.,0.,0.));
#17712=DIRECTION('center_axis',(1.,0.,0.));
#17713=DIRECTION('ref_axis',(0.,0.,-1.));
#17714=DIRECTION('',(-1.,0.,0.));
#17715=DIRECTION('center_axis',(1.,0.,0.));
#17716=DIRECTION('ref_axis',(0.,0.,-1.));
#17717=DIRECTION('',(-1.,0.,0.));
#17718=DIRECTION('center_axis',(1.,0.,0.));
#17719=DIRECTION('ref_axis',(0.,0.,-1.));
#17720=DIRECTION('',(-1.,0.,0.));
#17721=DIRECTION('center_axis',(1.,0.,0.));
#17722=DIRECTION('ref_axis',(0.,0.,-1.));
#17723=DIRECTION('',(-1.,0.,0.));
#17724=DIRECTION('center_axis',(1.,0.,0.));
#17725=DIRECTION('ref_axis',(0.,0.,-1.));
#17726=DIRECTION('',(-1.,0.,0.));
#17727=DIRECTION('center_axis',(1.,0.,0.));
#17728=DIRECTION('ref_axis',(0.,0.,-1.));
#17729=DIRECTION('',(-1.,0.,0.));
#17730=DIRECTION('center_axis',(1.,0.,0.));
#17731=DIRECTION('ref_axis',(0.,0.,-1.));
#17732=DIRECTION('',(-1.,0.,0.));
#17733=DIRECTION('center_axis',(1.,0.,0.));
#17734=DIRECTION('ref_axis',(0.,0.,-1.));
#17735=DIRECTION('',(-1.,0.,0.));
#17736=DIRECTION('center_axis',(1.,0.,0.));
#17737=DIRECTION('ref_axis',(0.,0.,-1.));
#17738=DIRECTION('',(-1.,0.,0.));
#17739=DIRECTION('center_axis',(1.,0.,0.));
#17740=DIRECTION('ref_axis',(0.,0.,-1.));
#17741=DIRECTION('',(-1.,0.,0.));
#17742=DIRECTION('center_axis',(1.,0.,0.));
#17743=DIRECTION('ref_axis',(0.,0.,-1.));
#17744=DIRECTION('',(-1.,0.,0.));
#17745=DIRECTION('center_axis',(1.,0.,0.));
#17746=DIRECTION('ref_axis',(0.,0.,-1.));
#17747=DIRECTION('',(-1.,0.,0.));
#17748=DIRECTION('center_axis',(1.,0.,0.));
#17749=DIRECTION('ref_axis',(0.,0.,-1.));
#17750=DIRECTION('',(-1.,0.,0.));
#17751=DIRECTION('center_axis',(1.,0.,0.));
#17752=DIRECTION('ref_axis',(0.,-1.17203152359781E-12,-1.));
#17753=DIRECTION('',(1.,0.,0.));
#17754=DIRECTION('center_axis',(1.,0.,0.));
#17755=DIRECTION('ref_axis',(0.,-1.17203152359781E-12,-1.));
#17756=DIRECTION('center_axis',(1.,0.,0.));
#17757=DIRECTION('ref_axis',(0.,-1.17203152359781E-12,-1.));
#17758=DIRECTION('',(1.,0.,0.));
#17759=DIRECTION('center_axis',(1.,0.,0.));
#17760=DIRECTION('ref_axis',(0.,-1.17203152359781E-12,-1.));
#17761=DIRECTION('center_axis',(1.,0.,0.));
#17762=DIRECTION('ref_axis',(0.,-1.17203152359781E-12,-1.));
#17763=DIRECTION('',(1.,0.,0.));
#17764=DIRECTION('center_axis',(1.,0.,0.));
#17765=DIRECTION('ref_axis',(0.,-1.17203152359781E-12,-1.));
#17766=DIRECTION('',(1.,0.,0.));
#17767=DIRECTION('center_axis',(1.,0.,0.));
#17768=DIRECTION('ref_axis',(0.,-1.17203152359781E-12,-1.));
#17769=DIRECTION('',(1.,0.,0.));
#17770=DIRECTION('center_axis',(1.,0.,0.));
#17771=DIRECTION('ref_axis',(0.,-1.17203152359781E-12,-1.));
#17772=DIRECTION('',(1.,0.,0.));
#17773=DIRECTION('center_axis',(1.,0.,0.));
#17774=DIRECTION('ref_axis',(0.,-1.17203152359781E-12,-1.));
#17775=DIRECTION('',(1.,0.,0.));
#17776=DIRECTION('center_axis',(1.,0.,0.));
#17777=DIRECTION('ref_axis',(0.,-1.17203152359781E-12,-1.));
#17778=DIRECTION('',(1.,0.,0.));
#17779=DIRECTION('center_axis',(1.,0.,0.));
#17780=DIRECTION('ref_axis',(0.,-1.17203152359781E-12,-1.));
#17781=DIRECTION('',(1.,0.,0.));
#17782=DIRECTION('center_axis',(1.,0.,0.));
#17783=DIRECTION('ref_axis',(0.,-1.17203152359781E-12,-1.));
#17784=DIRECTION('',(1.,0.,0.));
#17785=DIRECTION('center_axis',(1.,0.,0.));
#17786=DIRECTION('ref_axis',(0.,-1.17203152359781E-12,-1.));
#17787=DIRECTION('',(1.,0.,0.));
#17788=DIRECTION('center_axis',(1.,0.,0.));
#17789=DIRECTION('ref_axis',(0.,-1.17203152359781E-12,-1.));
#17790=DIRECTION('',(1.,0.,0.));
#17791=DIRECTION('center_axis',(1.,0.,0.));
#17792=DIRECTION('ref_axis',(0.,-1.17203152359781E-12,-1.));
#17793=DIRECTION('',(1.,0.,0.));
#17794=DIRECTION('center_axis',(1.,0.,0.));
#17795=DIRECTION('ref_axis',(0.,-1.17203152359781E-12,-1.));
#17796=DIRECTION('',(1.,0.,0.));
#17797=DIRECTION('center_axis',(1.,0.,0.));
#17798=DIRECTION('ref_axis',(0.,-1.17203152359781E-12,-1.));
#17799=DIRECTION('',(1.,0.,0.));
#17800=DIRECTION('center_axis',(1.,0.,0.));
#17801=DIRECTION('ref_axis',(0.,-1.17203152359781E-12,-1.));
#17802=DIRECTION('',(1.,0.,0.));
#17803=DIRECTION('center_axis',(1.,0.,0.));
#17804=DIRECTION('ref_axis',(0.,-1.17203152359781E-12,-1.));
#17805=DIRECTION('',(1.,0.,0.));
#17806=DIRECTION('center_axis',(1.,0.,0.));
#17807=DIRECTION('ref_axis',(0.,-1.17203152359781E-12,-1.));
#17808=DIRECTION('',(1.,0.,0.));
#17809=DIRECTION('center_axis',(1.,0.,0.));
#17810=DIRECTION('ref_axis',(0.,-1.17203152359781E-12,-1.));
#17811=DIRECTION('',(1.,0.,0.));
#17812=DIRECTION('center_axis',(1.,0.,0.));
#17813=DIRECTION('ref_axis',(0.,-1.17203152359781E-12,-1.));
#17814=DIRECTION('',(1.,0.,0.));
#17815=DIRECTION('center_axis',(1.,0.,0.));
#17816=DIRECTION('ref_axis',(0.,-1.17203152359781E-12,-1.));
#17817=DIRECTION('',(1.,0.,0.));
#17818=DIRECTION('center_axis',(1.,0.,0.));
#17819=DIRECTION('ref_axis',(0.,-1.17203152359781E-12,-1.));
#17820=DIRECTION('',(1.,0.,0.));
#17821=DIRECTION('center_axis',(1.,0.,0.));
#17822=DIRECTION('ref_axis',(0.,-1.17203152359781E-12,-1.));
#17823=DIRECTION('',(1.,0.,0.));
#17824=DIRECTION('center_axis',(1.,0.,0.));
#17825=DIRECTION('ref_axis',(0.,-1.17203152359781E-12,-1.));
#17826=DIRECTION('',(1.,0.,0.));
#17827=DIRECTION('center_axis',(1.,0.,0.));
#17828=DIRECTION('ref_axis',(0.,-1.17203152359781E-12,-1.));
#17829=DIRECTION('',(1.,0.,0.));
#17830=DIRECTION('center_axis',(1.,0.,0.));
#17831=DIRECTION('ref_axis',(0.,-1.17203152359781E-12,-1.));
#17832=DIRECTION('',(1.,0.,0.));
#17833=DIRECTION('center_axis',(1.,0.,0.));
#17834=DIRECTION('ref_axis',(0.,-1.17203152359781E-12,-1.));
#17835=DIRECTION('',(1.,0.,0.));
#17836=DIRECTION('center_axis',(1.,0.,0.));
#17837=DIRECTION('ref_axis',(0.,-1.17203152359781E-12,-1.));
#17838=DIRECTION('',(1.,0.,0.));
#17839=DIRECTION('center_axis',(1.,0.,0.));
#17840=DIRECTION('ref_axis',(0.,-1.17203152359781E-12,-1.));
#17841=DIRECTION('',(1.,0.,0.));
#17842=DIRECTION('center_axis',(1.,0.,0.));
#17843=DIRECTION('ref_axis',(0.,-1.17203152359781E-12,-1.));
#17844=DIRECTION('',(1.,0.,0.));
#17845=DIRECTION('center_axis',(1.,0.,0.));
#17846=DIRECTION('ref_axis',(0.,-1.17203152359781E-12,-1.));
#17847=DIRECTION('',(1.,0.,0.));
#17848=DIRECTION('center_axis',(1.,0.,0.));
#17849=DIRECTION('ref_axis',(0.,-1.17203152359781E-12,-1.));
#17850=DIRECTION('',(1.,0.,0.));
#17851=DIRECTION('center_axis',(1.,0.,0.));
#17852=DIRECTION('ref_axis',(0.,-1.17203152359781E-12,-1.));
#17853=DIRECTION('',(1.,0.,0.));
#17854=DIRECTION('center_axis',(1.,0.,0.));
#17855=DIRECTION('ref_axis',(0.,-1.17203152359781E-12,-1.));
#17856=DIRECTION('',(1.,0.,0.));
#17857=DIRECTION('center_axis',(1.,0.,0.));
#17858=DIRECTION('ref_axis',(0.,-1.17203152359781E-12,-1.));
#17859=DIRECTION('',(1.,0.,0.));
#17860=DIRECTION('center_axis',(1.,0.,0.));
#17861=DIRECTION('ref_axis',(0.,-1.17203152359781E-12,-1.));
#17862=DIRECTION('',(1.,0.,0.));
#17863=DIRECTION('center_axis',(1.,0.,0.));
#17864=DIRECTION('ref_axis',(0.,-1.17203152359781E-12,-1.));
#17865=DIRECTION('',(1.,0.,0.));
#17866=DIRECTION('center_axis',(1.,0.,0.));
#17867=DIRECTION('ref_axis',(0.,-1.17203152359781E-12,-1.));
#17868=DIRECTION('',(1.,0.,0.));
#17869=DIRECTION('center_axis',(1.,0.,0.));
#17870=DIRECTION('ref_axis',(0.,-1.17203152359781E-12,-1.));
#17871=DIRECTION('',(1.,0.,0.));
#17872=DIRECTION('center_axis',(1.,0.,0.));
#17873=DIRECTION('ref_axis',(0.,-1.17203152359781E-12,-1.));
#17874=DIRECTION('',(1.,0.,0.));
#17875=DIRECTION('center_axis',(1.,0.,0.));
#17876=DIRECTION('ref_axis',(0.,-1.17203152359781E-12,-1.));
#17877=DIRECTION('',(1.,0.,0.));
#17878=DIRECTION('center_axis',(1.,0.,0.));
#17879=DIRECTION('ref_axis',(0.,-1.17203152359781E-12,-1.));
#17880=DIRECTION('',(1.,0.,0.));
#17881=DIRECTION('center_axis',(1.,0.,0.));
#17882=DIRECTION('ref_axis',(0.,-1.17203152359781E-12,-1.));
#17883=DIRECTION('',(1.,0.,0.));
#17884=DIRECTION('center_axis',(1.,0.,0.));
#17885=DIRECTION('ref_axis',(0.,-1.17203152359781E-12,-1.));
#17886=DIRECTION('',(1.,0.,0.));
#17887=DIRECTION('center_axis',(1.,0.,0.));
#17888=DIRECTION('ref_axis',(0.,-1.17203152359781E-12,-1.));
#17889=DIRECTION('',(1.,0.,0.));
#17890=DIRECTION('center_axis',(1.,0.,0.));
#17891=DIRECTION('ref_axis',(0.,-1.17203152359781E-12,-1.));
#17892=DIRECTION('',(1.,0.,0.));
#17893=DIRECTION('center_axis',(1.,0.,0.));
#17894=DIRECTION('ref_axis',(0.,-1.17203152359781E-12,-1.));
#17895=DIRECTION('',(1.,0.,0.));
#17896=DIRECTION('center_axis',(1.,0.,0.));
#17897=DIRECTION('ref_axis',(0.,-1.17203152359781E-12,-1.));
#17898=DIRECTION('',(1.,0.,0.));
#17899=DIRECTION('center_axis',(1.,0.,0.));
#17900=DIRECTION('ref_axis',(0.,-1.17203152359781E-12,-1.));
#17901=DIRECTION('',(1.,0.,0.));
#17902=DIRECTION('center_axis',(1.,0.,0.));
#17903=DIRECTION('ref_axis',(0.,-1.17203152359781E-12,-1.));
#17904=DIRECTION('',(1.,0.,0.));
#17905=DIRECTION('center_axis',(1.,0.,0.));
#17906=DIRECTION('ref_axis',(0.,-1.17203152359781E-12,-1.));
#17907=DIRECTION('',(1.,0.,0.));
#17908=DIRECTION('center_axis',(1.,0.,0.));
#17909=DIRECTION('ref_axis',(0.,-1.17203152359781E-12,-1.));
#17910=DIRECTION('',(1.,0.,0.));
#17911=DIRECTION('center_axis',(1.,0.,0.));
#17912=DIRECTION('ref_axis',(0.,-1.17203152359781E-12,-1.));
#17913=DIRECTION('',(1.,0.,0.));
#17914=DIRECTION('center_axis',(1.,0.,0.));
#17915=DIRECTION('ref_axis',(0.,-1.17203152359781E-12,-1.));
#17916=DIRECTION('',(1.,0.,0.));
#17917=DIRECTION('center_axis',(1.,0.,0.));
#17918=DIRECTION('ref_axis',(0.,-1.17203152359781E-12,-1.));
#17919=DIRECTION('',(1.,0.,0.));
#17920=DIRECTION('center_axis',(1.,0.,0.));
#17921=DIRECTION('ref_axis',(0.,-1.17203152359781E-12,-1.));
#17922=DIRECTION('',(1.,0.,0.));
#17923=DIRECTION('center_axis',(1.,0.,0.));
#17924=DIRECTION('ref_axis',(0.,-1.17203152359781E-12,-1.));
#17925=DIRECTION('',(1.,0.,0.));
#17926=DIRECTION('center_axis',(1.,0.,0.));
#17927=DIRECTION('ref_axis',(0.,-1.17203152359781E-12,-1.));
#17928=DIRECTION('',(1.,0.,0.));
#17929=DIRECTION('center_axis',(1.,0.,0.));
#17930=DIRECTION('ref_axis',(0.,-1.17203152359781E-12,-1.));
#17931=DIRECTION('',(1.,0.,0.));
#17932=DIRECTION('center_axis',(1.,0.,0.));
#17933=DIRECTION('ref_axis',(0.,-1.17203152359781E-12,-1.));
#17934=DIRECTION('',(1.,0.,0.));
#17935=DIRECTION('center_axis',(1.,0.,0.));
#17936=DIRECTION('ref_axis',(0.,-1.17203152359781E-12,-1.));
#17937=DIRECTION('',(1.,0.,0.));
#17938=DIRECTION('center_axis',(1.,0.,0.));
#17939=DIRECTION('ref_axis',(0.,-1.17203152359781E-12,-1.));
#17940=DIRECTION('',(1.,0.,0.));
#17941=DIRECTION('center_axis',(1.,0.,0.));
#17942=DIRECTION('ref_axis',(0.,-1.17203152359781E-12,-1.));
#17943=DIRECTION('',(1.,0.,0.));
#17944=DIRECTION('center_axis',(1.,0.,0.));
#17945=DIRECTION('ref_axis',(0.,0.,-1.));
#17946=DIRECTION('center_axis',(1.,0.,0.));
#17947=DIRECTION('ref_axis',(0.,0.,-1.));
#17948=DIRECTION('center_axis',(-1.,0.,0.));
#17949=DIRECTION('ref_axis',(0.,-1.17203152359781E-12,-1.));
#17950=DIRECTION('center_axis',(1.,0.,0.));
#17951=DIRECTION('ref_axis',(0.,0.,-1.));
#17952=DIRECTION('',(-1.,0.,0.));
#17953=DIRECTION('center_axis',(1.,0.,0.));
#17954=DIRECTION('ref_axis',(0.,0.,-1.));
#17955=DIRECTION('center_axis',(1.,0.,0.));
#17956=DIRECTION('ref_axis',(0.,0.,-1.));
#17957=DIRECTION('center_axis',(1.,0.,0.));
#17958=DIRECTION('ref_axis',(0.,-1.17203152359781E-12,-1.));
#17959=DIRECTION('center_axis',(0.,1.,0.));
#17960=DIRECTION('ref_axis',(0.,0.,1.));
#17961=DIRECTION('',(-1.,0.,0.));
#17962=DIRECTION('',(0.,0.,1.));
#17963=DIRECTION('',(1.,0.,0.));
#17964=DIRECTION('',(0.,0.,1.));
#17965=DIRECTION('center_axis',(1.,0.,0.));
#17966=DIRECTION('ref_axis',(0.,0.,-1.));
#17967=DIRECTION('center_axis',(-1.,0.,0.));
#17968=DIRECTION('ref_axis',(0.,0.,-1.));
#17969=DIRECTION('',(0.,-1.,0.));
#17970=DIRECTION('',(0.,0.,-1.));
#17971=DIRECTION('center_axis',(0.,0.,1.));
#17972=DIRECTION('ref_axis',(0.,-1.,0.));
#17973=DIRECTION('',(0.,-1.,0.));
#17974=DIRECTION('',(1.,0.,0.));
#17975=DIRECTION('center_axis',(0.,-1.,0.));
#17976=DIRECTION('ref_axis',(0.,0.,-1.));
#17977=DIRECTION('',(1.,0.,0.));
#17978=DIRECTION('',(0.,0.,-1.));
#17979=DIRECTION('center_axis',(1.,0.,0.));
#17980=DIRECTION('ref_axis',(0.,0.,-1.));
#17981=DIRECTION('center_axis',(1.,0.,0.));
#17982=DIRECTION('ref_axis',(0.,0.,-1.));
#17983=DIRECTION('center_axis',(1.,0.,0.));
#17984=DIRECTION('ref_axis',(0.,0.,-1.));
#17985=DIRECTION('center_axis',(1.,0.,0.));
#17986=DIRECTION('ref_axis',(0.,0.,-1.));
#17987=DIRECTION('',(-1.,0.,0.));
#17988=DIRECTION('center_axis',(-1.,0.,0.));
#17989=DIRECTION('ref_axis',(0.,0.,-1.));
#17990=DIRECTION('center_axis',(1.,0.,0.));
#17991=DIRECTION('ref_axis',(0.,0.,-1.));
#17992=DIRECTION('center_axis',(1.,0.,0.));
#17993=DIRECTION('ref_axis',(0.,0.,-1.));
#17994=DIRECTION('center_axis',(1.,0.,0.));
#17995=DIRECTION('ref_axis',(0.,0.,-1.));
#17996=DIRECTION('center_axis',(-1.,0.,0.));
#17997=DIRECTION('ref_axis',(0.,0.,-1.));
#17998=DIRECTION('center_axis',(1.,0.,0.));
#17999=DIRECTION('ref_axis',(0.,0.,-1.));
#18000=DIRECTION('center_axis',(1.,0.,0.));
#18001=DIRECTION('ref_axis',(0.,0.,-1.));
#18002=DIRECTION('',(-1.,0.,0.));
#18003=DIRECTION('center_axis',(1.,0.,0.));
#18004=DIRECTION('ref_axis',(0.,0.,-1.));
#18005=DIRECTION('center_axis',(1.,0.,0.));
#18006=DIRECTION('ref_axis',(0.,0.,-1.));
#18007=DIRECTION('axis',(0.,0.,1.));
#18008=DIRECTION('refdir',(1.,0.,0.));
#18009=DIRECTION('center_axis',(1.,0.,0.));
#18010=DIRECTION('ref_axis',(0.,0.,-1.));
#18011=DIRECTION('center_axis',(-1.,0.,0.));
#18012=DIRECTION('ref_axis',(0.,0.,-1.));
#18013=DIRECTION('',(-1.,0.,0.));
#18014=DIRECTION('center_axis',(-1.,0.,0.));
#18015=DIRECTION('ref_axis',(0.,0.,-1.));
#18016=DIRECTION('center_axis',(1.,0.,0.));
#18017=DIRECTION('ref_axis',(0.,0.,-1.));
#18018=DIRECTION('center_axis',(1.,0.,0.));
#18019=DIRECTION('ref_axis',(0.,0.,-1.));
#18020=DIRECTION('',(-1.,0.,0.));
#18021=DIRECTION('center_axis',(1.,0.,0.));
#18022=DIRECTION('ref_axis',(0.,0.,-1.));
#18023=DIRECTION('center_axis',(1.,0.,0.));
#18024=DIRECTION('ref_axis',(0.,0.,-1.));
#18025=DIRECTION('center_axis',(1.,0.,0.));
#18026=DIRECTION('ref_axis',(0.,0.,-1.));
#18027=DIRECTION('axis',(0.,0.,1.));
#18028=DIRECTION('refdir',(1.,0.,0.));
#18029=DIRECTION('center_axis',(0.,1.,0.));
#18030=DIRECTION('ref_axis',(1.,0.,0.));
#18031=DIRECTION('',(1.,0.,0.));
#18032=DIRECTION('center_axis',(0.,1.,0.));
#18033=DIRECTION('ref_axis',(1.,0.,0.));
#18034=DIRECTION('center_axis',(0.,1.,0.));
#18035=DIRECTION('ref_axis',(1.,0.,0.));
#18036=DIRECTION('center_axis',(0.,1.,0.));
#18037=DIRECTION('ref_axis',(1.,0.,0.));
#18038=DIRECTION('',(0.,1.,0.));
#18039=DIRECTION('center_axis',(0.,1.,0.));
#18040=DIRECTION('ref_axis',(1.,0.,0.));
#18041=DIRECTION('',(-1.,0.,0.));
#18042=DIRECTION('center_axis',(1.,0.,0.));
#18043=DIRECTION('ref_axis',(0.,0.,-1.));
#18044=DIRECTION('center_axis',(-1.,0.,0.));
#18045=DIRECTION('ref_axis',(0.,0.,-1.));
#18046=DIRECTION('',(-1.,0.,0.));
#18047=DIRECTION('center_axis',(-1.,0.,0.));
#18048=DIRECTION('ref_axis',(0.,0.,-1.));
#18049=DIRECTION('center_axis',(1.,0.,0.));
#18050=DIRECTION('ref_axis',(0.,0.,-1.));
#18051=DIRECTION('center_axis',(1.,0.,0.));
#18052=DIRECTION('ref_axis',(0.,0.,-1.));
#18053=DIRECTION('',(-1.,0.,0.));
#18054=DIRECTION('center_axis',(1.,0.,0.));
#18055=DIRECTION('ref_axis',(0.,0.,-1.));
#18056=DIRECTION('center_axis',(1.,0.,0.));
#18057=DIRECTION('ref_axis',(0.,0.,-1.));
#18058=DIRECTION('center_axis',(1.,0.,0.));
#18059=DIRECTION('ref_axis',(0.,0.,-1.));
#18060=DIRECTION('axis',(0.,0.,1.));
#18061=DIRECTION('refdir',(1.,0.,0.));
#18062=DIRECTION('center_axis',(1.,0.,0.));
#18063=DIRECTION('ref_axis',(0.,0.,-1.));
#18064=DIRECTION('center_axis',(1.,0.,0.));
#18065=DIRECTION('ref_axis',(0.,0.,-1.));
#18066=DIRECTION('',(1.,0.,0.));
#18067=DIRECTION('center_axis',(-1.,0.,0.));
#18068=DIRECTION('ref_axis',(0.,0.,-1.));
#18069=DIRECTION('center_axis',(0.,1.,0.));
#18070=DIRECTION('ref_axis',(1.,0.,0.));
#18071=DIRECTION('',(1.,0.,0.));
#18072=DIRECTION('center_axis',(0.,1.,0.));
#18073=DIRECTION('ref_axis',(1.,0.,0.));
#18074=DIRECTION('center_axis',(0.,1.,0.));
#18075=DIRECTION('ref_axis',(1.,0.,0.));
#18076=DIRECTION('center_axis',(0.,1.,0.));
#18077=DIRECTION('ref_axis',(1.,0.,0.));
#18078=DIRECTION('',(0.,1.,0.));
#18079=DIRECTION('center_axis',(0.,1.,0.));
#18080=DIRECTION('ref_axis',(1.,0.,0.));
#18081=DIRECTION('',(-1.,0.,0.));
#18082=DIRECTION('center_axis',(0.,-1.,0.));
#18083=DIRECTION('ref_axis',(0.,0.,-1.));
#18084=DIRECTION('',(0.,0.,1.));
#18085=DIRECTION('',(1.,0.,0.));
#18086=DIRECTION('',(0.,0.,-1.));
#18087=DIRECTION('',(1.,0.,0.));
#18088=DIRECTION('',(0.,0.,-1.));
#18089=DIRECTION('',(-1.,0.,0.));
#18090=DIRECTION('center_axis',(0.,0.,-1.));
#18091=DIRECTION('ref_axis',(0.,1.,0.));
#18092=DIRECTION('',(0.,-1.,0.));
#18093=DIRECTION('',(1.,0.,0.));
#18094=DIRECTION('',(0.,1.,0.));
#18095=DIRECTION('center_axis',(0.,1.,0.));
#18096=DIRECTION('ref_axis',(0.,0.,1.));
#18097=DIRECTION('',(0.,0.,-1.));
#18098=DIRECTION('',(1.,0.,0.));
#18099=DIRECTION('',(0.,0.,1.));
#18100=DIRECTION('',(-1.,0.,0.));
#18101=DIRECTION('',(0.,0.,1.));
#18102=DIRECTION('center_axis',(1.,0.,0.));
#18103=DIRECTION('ref_axis',(0.,0.,-1.));
#18104=DIRECTION('center_axis',(1.,0.,0.));
#18105=DIRECTION('ref_axis',(0.,0.,-1.));
#18106=DIRECTION('center_axis',(-1.,0.,0.));
#18107=DIRECTION('ref_axis',(0.,0.,-1.));
#18108=DIRECTION('center_axis',(1.,0.,0.));
#18109=DIRECTION('ref_axis',(0.,0.,-1.));
#18110=DIRECTION('center_axis',(1.,0.,0.));
#18111=DIRECTION('ref_axis',(0.,0.,-1.));
#18112=DIRECTION('center_axis',(1.,0.,0.));
#18113=DIRECTION('ref_axis',(0.,0.,-1.));
#18114=DIRECTION('center_axis',(1.,0.,0.));
#18115=DIRECTION('ref_axis',(0.,0.,-1.));
#18116=DIRECTION('',(-1.,0.,0.));
#18117=DIRECTION('center_axis',(1.,0.,0.));
#18118=DIRECTION('ref_axis',(0.,1.22464679914735E-16,1.));
#18119=DIRECTION('center_axis',(-1.,0.,0.));
#18120=DIRECTION('ref_axis',(0.,0.,-1.));
#18121=DIRECTION('center_axis',(1.,0.,0.));
#18122=DIRECTION('ref_axis',(0.,1.22464679914735E-16,1.));
#18123=DIRECTION('center_axis',(1.,0.,0.));
#18124=DIRECTION('ref_axis',(0.,0.,-1.));
#18125=DIRECTION('center_axis',(1.,0.,0.));
#18126=DIRECTION('ref_axis',(0.,0.,-1.));
#18127=DIRECTION('axis',(0.,0.,1.));
#18128=DIRECTION('refdir',(1.,0.,0.));
#18129=DIRECTION('center_axis',(1.,0.,0.));
#18130=DIRECTION('ref_axis',(0.,0.,-1.));
#18131=DIRECTION('center_axis',(-1.,0.,0.));
#18132=DIRECTION('ref_axis',(0.,0.,-1.));
#18133=DIRECTION('',(-1.,0.,0.));
#18134=DIRECTION('center_axis',(-1.,0.,0.));
#18135=DIRECTION('ref_axis',(0.,0.,-1.));
#18136=DIRECTION('center_axis',(1.,0.,0.));
#18137=DIRECTION('ref_axis',(0.,0.,-1.));
#18138=DIRECTION('center_axis',(1.,0.,0.));
#18139=DIRECTION('ref_axis',(0.,0.,-1.));
#18140=DIRECTION('',(-1.,0.,0.));
#18141=DIRECTION('center_axis',(1.,0.,0.));
#18142=DIRECTION('ref_axis',(0.,0.,-1.));
#18143=DIRECTION('center_axis',(1.,0.,0.));
#18144=DIRECTION('ref_axis',(0.,0.,-1.));
#18145=DIRECTION('center_axis',(1.,0.,0.));
#18146=DIRECTION('ref_axis',(0.,0.,-1.));
#18147=DIRECTION('axis',(0.,0.,1.));
#18148=DIRECTION('refdir',(1.,0.,0.));
#18149=DIRECTION('center_axis',(1.,0.,0.));
#18150=DIRECTION('ref_axis',(0.,0.,-1.));
#18151=DIRECTION('center_axis',(-1.,0.,0.));
#18152=DIRECTION('ref_axis',(0.,0.,-1.));
#18153=DIRECTION('',(-1.,0.,0.));
#18154=DIRECTION('center_axis',(-1.,0.,0.));
#18155=DIRECTION('ref_axis',(0.,0.,-1.));
#18156=DIRECTION('center_axis',(1.,0.,0.));
#18157=DIRECTION('ref_axis',(0.,0.,-1.));
#18158=DIRECTION('center_axis',(1.,0.,0.));
#18159=DIRECTION('ref_axis',(0.,0.,-1.));
#18160=DIRECTION('',(-1.,0.,0.));
#18161=DIRECTION('center_axis',(1.,0.,0.));
#18162=DIRECTION('ref_axis',(0.,0.,-1.));
#18163=DIRECTION('center_axis',(1.,0.,0.));
#18164=DIRECTION('ref_axis',(0.,0.,-1.));
#18165=DIRECTION('center_axis',(1.,0.,0.));
#18166=DIRECTION('ref_axis',(0.,0.,-1.));
#18167=DIRECTION('axis',(0.,0.,1.));
#18168=DIRECTION('refdir',(1.,0.,0.));
#18169=DIRECTION('center_axis',(1.,0.,0.));
#18170=DIRECTION('ref_axis',(0.,0.,-1.));
#18171=DIRECTION('',(0.,-0.707106781186547,-0.707106781186548));
#18172=DIRECTION('',(0.,-1.,0.));
#18173=DIRECTION('',(0.,-0.707106781186547,0.707106781186548));
#18174=DIRECTION('',(0.,0.,1.));
#18175=DIRECTION('',(0.,0.707106781186547,0.707106781186548));
#18176=DIRECTION('',(0.,1.,0.));
#18177=DIRECTION('',(0.,0.707106781186547,-0.707106781186548));
#18178=DIRECTION('',(0.,0.,-1.));
#18179=DIRECTION('center_axis',(0.,0.707106781186548,-0.707106781186547));
#18180=DIRECTION('ref_axis',(-1.,0.,0.));
#18181=DIRECTION('',(1.,0.,0.));
#18182=DIRECTION('',(0.,-0.707106781186547,-0.707106781186548));
#18183=DIRECTION('',(-1.,0.,0.));
#18184=DIRECTION('center_axis',(0.,1.,0.));
#18185=DIRECTION('ref_axis',(-1.,0.,0.));
#18186=DIRECTION('',(-1.,0.,0.));
#18187=DIRECTION('',(0.,0.,-1.));
#18188=DIRECTION('center_axis',(0.,0.707106781186548,0.707106781186547));
#18189=DIRECTION('ref_axis',(1.,0.,0.));
#18190=DIRECTION('',(1.,0.,0.));
#18191=DIRECTION('',(0.,0.707106781186547,-0.707106781186548));
#18192=DIRECTION('center_axis',(0.,0.,1.));
#18193=DIRECTION('ref_axis',(1.,0.,0.));
#18194=DIRECTION('',(-1.,0.,0.));
#18195=DIRECTION('',(0.,1.,0.));
#18196=DIRECTION('center_axis',(1.,0.,0.));
#18197=DIRECTION('ref_axis',(0.,0.,-1.));
#18198=DIRECTION('',(0.,-0.707106781186547,0.707106781186548));
#18199=DIRECTION('',(0.,-1.,0.));
#18200=DIRECTION('',(0.,0.707106781186547,0.707106781186548));
#18201=DIRECTION('',(0.,0.,1.));
#18202=DIRECTION('center_axis',(0.,0.,1.));
#18203=DIRECTION('ref_axis',(1.,0.,0.));
#18204=DIRECTION('',(1.,0.,0.));
#18205=DIRECTION('center_axis',(0.,-0.707106781186548,0.707106781186547));
#18206=DIRECTION('ref_axis',(1.,0.,0.));
#18207=DIRECTION('',(1.,0.,0.));
#18208=DIRECTION('center_axis',(0.,-0.707106781186548,-0.707106781186547));
#18209=DIRECTION('ref_axis',(-1.,0.,0.));
#18210=DIRECTION('',(-1.,0.,0.));
#18211=DIRECTION('center_axis',(0.,-1.,0.));
#18212=DIRECTION('ref_axis',(1.,0.,0.));
#18213=DIRECTION('axis',(0.,0.,1.));
#18214=DIRECTION('refdir',(1.,0.,0.));
#18215=DIRECTION('center_axis',(0.866025403784439,0.,-0.5));
#18216=DIRECTION('ref_axis',(0.5,0.,0.866025403784439));
#18217=DIRECTION('',(0.5,0.,0.866025403784439));
#18218=DIRECTION('',(0.,-1.,0.));
#18219=DIRECTION('',(0.5,0.,0.866025403784439));
#18220=DIRECTION('',(0.,-1.,0.));
#18221=DIRECTION('center_axis',(1.92296268638356E-16,0.,-1.));
#18222=DIRECTION('ref_axis',(1.,0.,1.92296268638356E-16));
#18223=DIRECTION('',(1.,0.,1.92296268638356E-16));
#18224=DIRECTION('',(0.,-1.,0.));
#18225=DIRECTION('',(1.,0.,1.92296268638356E-16));
#18226=DIRECTION('center_axis',(-0.866025403784439,0.,-0.5));
#18227=DIRECTION('ref_axis',(0.5,0.,-0.866025403784439));
#18228=DIRECTION('',(0.5,0.,-0.866025403784439));
#18229=DIRECTION('',(0.,-1.,0.));
#18230=DIRECTION('',(0.5,0.,-0.866025403784438));
#18231=DIRECTION('center_axis',(-0.866025403784439,0.,0.5));
#18232=DIRECTION('ref_axis',(-0.5,0.,-0.866025403784439));
#18233=DIRECTION('',(-0.5,0.,-0.866025403784439));
#18234=DIRECTION('',(0.,-1.,0.));
#18235=DIRECTION('',(-0.5,0.,-0.866025403784439));
#18236=DIRECTION('center_axis',(-1.92296268638356E-16,0.,1.));
#18237=DIRECTION('ref_axis',(-1.,0.,-1.92296268638356E-16));
#18238=DIRECTION('',(-1.,0.,-1.92296268638356E-16));
#18239=DIRECTION('',(0.,-1.,0.));
#18240=DIRECTION('',(-1.,0.,-1.92296268638356E-16));
#18241=DIRECTION('center_axis',(0.866025403784439,0.,0.5));
#18242=DIRECTION('ref_axis',(-0.5,0.,0.866025403784439));
#18243=DIRECTION('',(-0.5,0.,0.866025403784439));
#18244=DIRECTION('',(-0.5,0.,0.866025403784439));
#18245=DIRECTION('center_axis',(0.,-1.,0.));
#18246=DIRECTION('ref_axis',(0.,0.,-1.));
#18247=DIRECTION('center_axis',(0.,1.,0.));
#18248=DIRECTION('ref_axis',(0.,0.,1.));
#18249=DIRECTION('center_axis',(0.,-1.,0.));
#18250=DIRECTION('ref_axis',(1.,0.,0.));
#18251=DIRECTION('center_axis',(0.,-1.,0.));
#18252=DIRECTION('ref_axis',(1.,0.,0.));
#18253=DIRECTION('center_axis',(0.,-1.,0.));
#18254=DIRECTION('ref_axis',(1.,0.,0.));
#18255=DIRECTION('',(0.707106781186547,0.707106781186548,8.65956056235493E-17));
#18256=DIRECTION('center_axis',(0.,-1.,0.));
#18257=DIRECTION('ref_axis',(1.,0.,0.));
#18258=DIRECTION('center_axis',(0.,1.,0.));
#18259=DIRECTION('ref_axis',(1.,0.,0.));
#18260=DIRECTION('',(0.,1.,0.));
#18261=DIRECTION('center_axis',(0.,1.,0.));
#18262=DIRECTION('ref_axis',(1.,0.,0.));
#18263=DIRECTION('center_axis',(0.,-1.,0.));
#18264=DIRECTION('ref_axis',(1.,0.,0.));
#18265=DIRECTION('',(-0.707106781186547,0.707106781186548,-8.65956056235493E-17));
#18266=DIRECTION('center_axis',(0.,-1.,0.));
#18267=DIRECTION('ref_axis',(0.,0.,-1.));
#18268=DIRECTION('axis',(0.,0.,1.));
#18269=DIRECTION('refdir',(1.,0.,0.));
#18270=DIRECTION('center_axis',(0.,1.,0.));
#18271=DIRECTION('ref_axis',(1.,0.,0.));
#18272=DIRECTION('center_axis',(0.,-1.,0.));
#18273=DIRECTION('ref_axis',(1.,0.,0.));
#18274=DIRECTION('',(0.,-1.,0.));
#18275=DIRECTION('center_axis',(0.,-1.,0.));
#18276=DIRECTION('ref_axis',(1.,0.,0.));
#18277=DIRECTION('center_axis',(0.,1.,0.));
#18278=DIRECTION('ref_axis',(1.,0.,0.));
#18279=DIRECTION('center_axis',(0.,1.,0.));
#18280=DIRECTION('ref_axis',(1.,0.,0.));
#18281=DIRECTION('',(0.,-1.,0.));
#18282=DIRECTION('center_axis',(0.,1.,0.));
#18283=DIRECTION('ref_axis',(1.,0.,0.));
#18284=DIRECTION('center_axis',(0.,1.,0.));
#18285=DIRECTION('ref_axis',(1.,0.,0.));
#18286=DIRECTION('center_axis',(0.,1.,0.));
#18287=DIRECTION('ref_axis',(1.,0.,0.));
#18288=DIRECTION('axis',(0.,0.,1.));
#18289=DIRECTION('refdir',(1.,0.,0.));
#18290=DIRECTION('center_axis',(0.,1.,0.));
#18291=DIRECTION('ref_axis',(0.,0.,1.));
#18292=DIRECTION('center_axis',(0.,-1.,0.));
#18293=DIRECTION('ref_axis',(1.,0.,0.));
#18294=DIRECTION('center_axis',(0.,-1.,0.));
#18295=DIRECTION('ref_axis',(1.,0.,0.));
#18296=DIRECTION('center_axis',(0.,-1.,0.));
#18297=DIRECTION('ref_axis',(1.,0.,0.));
#18298=DIRECTION('',(0.707106781186548,0.707106781186547,8.65956056235494E-17));
#18299=DIRECTION('center_axis',(0.,-1.,0.));
#18300=DIRECTION('ref_axis',(1.,0.,0.));
#18301=DIRECTION('center_axis',(0.,-1.,0.));
#18302=DIRECTION('ref_axis',(1.,0.,0.));
#18303=DIRECTION('',(0.,1.,0.));
#18304=DIRECTION('center_axis',(0.,1.,0.));
#18305=DIRECTION('ref_axis',(1.,0.,0.));
#18306=DIRECTION('center_axis',(0.,-1.,0.));
#18307=DIRECTION('ref_axis',(1.,0.,0.));
#18308=DIRECTION('',(-0.707106781186547,0.707106781186548,-8.65956056235493E-17));
#18309=DIRECTION('center_axis',(0.,-1.,0.));
#18310=DIRECTION('ref_axis',(0.,0.,-1.));
#18311=DIRECTION('center_axis',(0.,-1.,0.));
#18312=DIRECTION('ref_axis',(1.,0.,0.));
#18313=DIRECTION('center_axis',(0.,1.,0.));
#18314=DIRECTION('ref_axis',(1.,0.,0.));
#18315=DIRECTION('center_axis',(0.,1.,0.));
#18316=DIRECTION('ref_axis',(1.,0.,0.));
#18317=DIRECTION('',(-0.447213595499958,0.894427190999916,-5.47678698264203E-17));
#18318=DIRECTION('center_axis',(0.,-1.,0.));
#18319=DIRECTION('ref_axis',(1.,0.,0.));
#18320=DIRECTION('center_axis',(0.,1.,0.));
#18321=DIRECTION('ref_axis',(1.,0.,0.));
#18322=DIRECTION('',(0.,1.,0.));
#18323=DIRECTION('center_axis',(0.,1.,0.));
#18324=DIRECTION('ref_axis',(1.,0.,0.));
#18325=DIRECTION('center_axis',(0.,-1.,0.));
#18326=DIRECTION('ref_axis',(1.,0.,0.));
#18327=DIRECTION('',(-0.707106781186547,0.707106781186548,-8.65956056235493E-17));
#18328=DIRECTION('center_axis',(0.,-1.,0.));
#18329=DIRECTION('ref_axis',(0.,0.,-1.));
#18330=DIRECTION('center_axis',(0.866025403784439,0.,-0.5));
#18331=DIRECTION('ref_axis',(0.5,0.,0.866025403784439));
#18332=DIRECTION('',(-0.5,0.,-0.866025403784439));
#18333=DIRECTION('',(0.,-1.,0.));
#18334=DIRECTION('',(0.5,0.,0.866025403784439));
#18335=DIRECTION('',(0.,-1.,0.));
#18336=DIRECTION('center_axis',(1.92296268638356E-16,0.,-1.));
#18337=DIRECTION('ref_axis',(1.,0.,1.92296268638356E-16));
#18338=DIRECTION('',(-1.,0.,-1.92296268638356E-16));
#18339=DIRECTION('',(0.,-1.,0.));
#18340=DIRECTION('',(1.,0.,1.92296268638356E-16));
#18341=DIRECTION('center_axis',(-0.866025403784439,0.,-0.5));
#18342=DIRECTION('ref_axis',(0.5,0.,-0.866025403784439));
#18343=DIRECTION('',(-0.5,0.,0.866025403784438));
#18344=DIRECTION('',(0.,-1.,0.));
#18345=DIRECTION('',(0.5,0.,-0.866025403784438));
#18346=DIRECTION('center_axis',(-0.866025403784439,0.,0.5));
#18347=DIRECTION('ref_axis',(-0.5,0.,-0.866025403784439));
#18348=DIRECTION('',(0.5,0.,0.866025403784439));
#18349=DIRECTION('',(0.,-1.,0.));
#18350=DIRECTION('',(-0.5,0.,-0.866025403784439));
#18351=DIRECTION('center_axis',(-1.92296268638356E-16,0.,1.));
#18352=DIRECTION('ref_axis',(-1.,0.,-1.92296268638356E-16));
#18353=DIRECTION('',(1.,0.,1.92296268638356E-16));
#18354=DIRECTION('',(0.,-1.,0.));
#18355=DIRECTION('',(-1.,0.,-1.92296268638356E-16));
#18356=DIRECTION('center_axis',(0.866025403784439,0.,0.5));
#18357=DIRECTION('ref_axis',(-0.5,0.,0.866025403784439));
#18358=DIRECTION('',(0.5,0.,-0.866025403784439));
#18359=DIRECTION('',(-0.5,0.,0.866025403784439));
#18360=DIRECTION('center_axis',(0.,1.,0.));
#18361=DIRECTION('ref_axis',(1.,0.,0.));
#18362=DIRECTION('center_axis',(0.,-1.,0.));
#18363=DIRECTION('ref_axis',(0.,0.,-1.));
#18364=DIRECTION('',(0.,0.,1.));
#18365=DIRECTION('',(1.,0.,0.));
#18366=DIRECTION('',(0.,0.,1.));
#18367=DIRECTION('',(1.,0.,0.));
#18368=DIRECTION('',(0.,0.,1.));
#18369=DIRECTION('',(1.,0.,0.));
#18370=DIRECTION('',(0.,0.,1.));
#18371=DIRECTION('',(1.,0.,0.));
#18372=DIRECTION('',(0.,0.,1.));
#18373=DIRECTION('',(1.,0.,0.));
#18374=DIRECTION('',(0.,0.,1.));
#18375=DIRECTION('',(1.,0.,0.));
#18376=DIRECTION('',(0.,0.,1.));
#18377=DIRECTION('',(1.,0.,0.));
#18378=DIRECTION('',(0.,0.,1.));
#18379=DIRECTION('',(1.,0.,0.));
#18380=DIRECTION('',(0.,-1.,2.22044604925031E-16));
#18381=DIRECTION('',(1.,0.,0.));
#18382=DIRECTION('',(0.,-1.,2.22044604925031E-16));
#18383=DIRECTION('',(1.,0.,0.));
#18384=DIRECTION('',(0.,-1.,2.22044604925031E-16));
#18385=DIRECTION('',(1.,0.,0.));
#18386=DIRECTION('',(0.,-1.,2.22044604925031E-16));
#18387=DIRECTION('',(1.,0.,0.));
#18388=DIRECTION('',(0.,0.,1.));
#18389=DIRECTION('',(1.,0.,0.));
#18390=DIRECTION('',(0.,-1.,2.22044604925031E-16));
#18391=DIRECTION('',(1.,0.,0.));
#18392=DIRECTION('',(0.,-1.,2.22044604925031E-16));
#18393=DIRECTION('',(1.,0.,0.));
#18394=DIRECTION('',(0.,-1.,2.22044604925031E-16));
#18395=DIRECTION('',(1.,0.,0.));
#18396=DIRECTION('',(0.,-1.,2.22044604925031E-16));
#18397=DIRECTION('',(1.,0.,0.));
#18398=DIRECTION('',(0.,1.,2.22044604925031E-16));
#18399=DIRECTION('',(1.,0.,0.));
#18400=DIRECTION('',(0.,1.,2.22044604925031E-16));
#18401=DIRECTION('',(1.,0.,0.));
#18402=DIRECTION('',(0.,0.,1.));
#18403=DIRECTION('',(2.22044604925031E-16,-1.,0.));
#18404=DIRECTION('',(0.,0.,1.));
#18405=DIRECTION('',(2.22044604925031E-16,1.,0.));
#18406=DIRECTION('',(0.,0.,1.));
#18407=DIRECTION('',(2.22044604925031E-16,1.,0.));
#18408=DIRECTION('',(0.,0.,1.));
#18409=DIRECTION('',(2.22044604925031E-16,1.,0.));
#18410=DIRECTION('',(0.,1.,2.22044604925031E-16));
#18411=DIRECTION('',(1.,0.,0.));
#18412=DIRECTION('',(0.,1.,2.22044604925031E-16));
#18413=DIRECTION('',(1.,0.,0.));
#18414=DIRECTION('',(0.,0.,1.));
#18415=DIRECTION('',(2.22044604925031E-16,-1.,0.));
#18416=DIRECTION('',(0.,0.,1.));
#18417=DIRECTION('',(2.22044604925031E-16,-1.,0.));
#18418=DIRECTION('',(0.,0.,1.));
#18419=DIRECTION('',(2.22044604925031E-16,-1.,0.));
#18420=DIRECTION('',(0.,0.,1.));
#18421=DIRECTION('',(2.22044604925031E-16,-1.,0.));
#18422=DIRECTION('',(0.,-1.,2.22044604925031E-16));
#18423=DIRECTION('',(1.,0.,0.));
#18424=DIRECTION('',(0.,-1.,2.22044604925031E-16));
#18425=DIRECTION('',(1.,0.,0.));
#18426=DIRECTION('',(0.,-1.,2.22044604925031E-16));
#18427=DIRECTION('',(1.,0.,0.));
#18428=DIRECTION('',(0.,-1.,2.22044604925031E-16));
#18429=DIRECTION('',(1.,0.,0.));
#18430=DIRECTION('',(0.,0.,1.));
#18431=DIRECTION('',(1.,0.,0.));
#18432=DIRECTION('',(0.,0.,1.));
#18433=DIRECTION('',(1.,0.,0.));
#18434=DIRECTION('',(0.,-1.,2.22044604925031E-16));
#18435=DIRECTION('',(1.,0.,0.));
#18436=DIRECTION('',(0.,-1.,2.22044604925031E-16));
#18437=DIRECTION('',(1.,0.,0.));
#18438=DIRECTION('',(0.,0.,1.));
#18439=DIRECTION('',(1.,0.,0.));
#18440=DIRECTION('',(0.,-1.,2.22044604925031E-16));
#18441=DIRECTION('',(1.,0.,0.));
#18442=DIRECTION('',(0.,-1.,2.22044604925031E-16));
#18443=DIRECTION('',(1.,0.,0.));
#18444=DIRECTION('',(0.,0.,1.));
#18445=DIRECTION('',(1.,0.,0.));
#18446=DIRECTION('',(0.,0.,1.));
#18447=DIRECTION('',(1.,0.,0.));
#18448=DIRECTION('',(0.,-1.,2.22044604925031E-16));
#18449=DIRECTION('',(1.,0.,0.));
#18450=DIRECTION('',(0.,-1.,2.22044604925031E-16));
#18451=DIRECTION('',(1.,0.,0.));
#18452=DIRECTION('',(0.,0.,1.));
#18453=DIRECTION('',(1.,0.,0.));
#18454=DIRECTION('',(0.,-1.,2.22044604925031E-16));
#18455=DIRECTION('',(1.,0.,0.));
#18456=DIRECTION('',(0.,-1.,2.22044604925031E-16));
#18457=DIRECTION('',(1.,0.,0.));
#18458=DIRECTION('',(0.,0.,1.));
#18459=DIRECTION('',(1.,0.,0.));
#18460=DIRECTION('',(0.,0.,1.));
#18461=DIRECTION('',(1.,0.,0.));
#18462=DIRECTION('',(0.,0.,1.));
#18463=DIRECTION('',(1.,0.,0.));
#18464=DIRECTION('',(0.,0.,1.));
#18465=DIRECTION('',(1.,0.,0.));
#18466=DIRECTION('',(0.,0.,1.));
#18467=DIRECTION('',(1.,0.,0.));
#18468=DIRECTION('',(0.,0.,1.));
#18469=DIRECTION('',(1.,0.,0.));
#18470=DIRECTION('',(0.,-1.22464679914735E-16,-1.));
#18471=DIRECTION('',(1.,0.,0.));
#18472=DIRECTION('',(0.,0.,1.));
#18473=DIRECTION('',(1.,0.,0.));
#18474=DIRECTION('',(0.,0.,1.));
#18475=DIRECTION('',(1.,0.,0.));
#18476=DIRECTION('',(0.,0.,1.));
#18477=DIRECTION('',(2.22044604925031E-16,-1.,0.));
#18478=DIRECTION('',(0.,0.,1.));
#18479=DIRECTION('',(2.22044604925031E-16,-1.,0.));
#18480=DIRECTION('',(0.,0.,1.));
#18481=DIRECTION('',(1.,0.,0.));
#18482=DIRECTION('',(6.12323399573677E-17,-6.12323399573677E-17,1.));
#18483=DIRECTION('',(1.,6.12323399573677E-17,-6.12323399573677E-17));
#18484=DIRECTION('',(0.,0.172766500737384,0.984962809563366));
#18485=DIRECTION('',(1.,0.,0.));
#18486=CARTESIAN_POINT('',(0.,0.,0.));
#18487=CARTESIAN_POINT('',(0.,0.,0.));
#18488=CARTESIAN_POINT('',(0.,0.,0.));
#18489=CARTESIAN_POINT('Origin',(19.,-9.,-0.1));
#18490=CARTESIAN_POINT('',(18.725,-9.,0.));
#18491=CARTESIAN_POINT('Origin',(19.,-9.,0.));
#18492=CARTESIAN_POINT('',(18.725,-9.,1.2));
#18493=CARTESIAN_POINT('',(18.725,-9.,-0.1));
#18494=CARTESIAN_POINT('Origin',(19.,-9.,1.2));
#18495=CARTESIAN_POINT('Origin',(8.,-0.9,-0.1));
#18496=CARTESIAN_POINT('',(7.725,-0.9,0.));
#18497=CARTESIAN_POINT('Origin',(8.,-0.9,0.));
#18498=CARTESIAN_POINT('',(7.725,-0.9,1.2));
#18499=CARTESIAN_POINT('',(7.725,-0.9,-0.1));
#18500=CARTESIAN_POINT('Origin',(8.,-0.9,1.2));
#18501=CARTESIAN_POINT('Origin',(8.,-9.,-0.1));
#18502=CARTESIAN_POINT('',(7.725,-9.,0.));
#18503=CARTESIAN_POINT('Origin',(8.,-9.,0.));
#18504=CARTESIAN_POINT('',(7.725,-9.,1.2));
#18505=CARTESIAN_POINT('',(7.725,-9.,-0.1));
#18506=CARTESIAN_POINT('Origin',(8.,-9.,1.2));
#18507=CARTESIAN_POINT('Origin',(19.,-0.9,-0.1));
#18508=CARTESIAN_POINT('',(18.725,-0.9,0.));
#18509=CARTESIAN_POINT('Origin',(19.,-0.9,0.));
#18510=CARTESIAN_POINT('',(18.725,-0.9,1.2));
#18511=CARTESIAN_POINT('',(18.725,-0.9,-0.1));
#18512=CARTESIAN_POINT('Origin',(19.,-0.9,1.2));
#18513=CARTESIAN_POINT('Origin',(22.3,-9.,-0.1));
#18514=CARTESIAN_POINT('',(22.09,-9.,0.));
#18515=CARTESIAN_POINT('Origin',(22.3,-9.,0.));
#18516=CARTESIAN_POINT('',(22.09,-9.,1.2));
#18517=CARTESIAN_POINT('',(22.09,-9.,-0.1));
#18518=CARTESIAN_POINT('Origin',(22.3,-9.,1.2));
#18519=CARTESIAN_POINT('Origin',(22.3,-3.,-0.1));
#18520=CARTESIAN_POINT('',(22.09,-3.,0.));
#18521=CARTESIAN_POINT('Origin',(22.3,-3.,0.));
#18522=CARTESIAN_POINT('',(22.09,-3.,1.2));
#18523=CARTESIAN_POINT('',(22.09,-3.,-0.1));
#18524=CARTESIAN_POINT('Origin',(22.3,-3.,1.2));
#18525=CARTESIAN_POINT('Origin',(4.7,-9.,-0.1));
#18526=CARTESIAN_POINT('',(4.49,-9.,0.));
#18527=CARTESIAN_POINT('Origin',(4.7,-9.,0.));
#18528=CARTESIAN_POINT('',(4.49,-9.,1.2));
#18529=CARTESIAN_POINT('',(4.49,-9.,-0.1));
#18530=CARTESIAN_POINT('Origin',(4.7,-9.,1.2));
#18531=CARTESIAN_POINT('Origin',(4.7,-3.,-0.1));
#18532=CARTESIAN_POINT('',(4.49,-3.,0.));
#18533=CARTESIAN_POINT('Origin',(4.7,-3.,0.));
#18534=CARTESIAN_POINT('',(4.49,-3.,1.2));
#18535=CARTESIAN_POINT('',(4.49,-3.,-0.1));
#18536=CARTESIAN_POINT('Origin',(4.7,-3.,1.2));
#18537=CARTESIAN_POINT('Origin',(24.,-3.5,-0.1));
#18538=CARTESIAN_POINT('',(23.67,-3.5,0.));
#18539=CARTESIAN_POINT('Origin',(24.,-3.5,0.));
#18540=CARTESIAN_POINT('',(23.67,-3.5,1.2));
#18541=CARTESIAN_POINT('',(23.67,-3.5,-0.1));
#18542=CARTESIAN_POINT('Origin',(24.,-3.5,1.2));
#18543=CARTESIAN_POINT('Origin',(24.,3.5,-0.1));
#18544=CARTESIAN_POINT('',(23.67,3.5,0.));
#18545=CARTESIAN_POINT('Origin',(24.,3.5,0.));
#18546=CARTESIAN_POINT('',(23.67,3.5,1.2));
#18547=CARTESIAN_POINT('',(23.67,3.5,-0.1));
#18548=CARTESIAN_POINT('Origin',(24.,3.5,1.2));
#18549=CARTESIAN_POINT('Origin',(3.,-2.4,-0.1));
#18550=CARTESIAN_POINT('',(2.725,-2.4,0.));
#18551=CARTESIAN_POINT('Origin',(3.,-2.4,0.));
#18552=CARTESIAN_POINT('',(2.725,-2.4,1.2));
#18553=CARTESIAN_POINT('',(2.725,-2.4,-0.1));
#18554=CARTESIAN_POINT('Origin',(3.,-2.4,1.2));
#18555=CARTESIAN_POINT('Origin',(3.,2.4,-0.1));
#18556=CARTESIAN_POINT('',(2.725,2.4,0.));
#18557=CARTESIAN_POINT('Origin',(3.,2.4,0.));
#18558=CARTESIAN_POINT('',(2.725,2.4,1.2));
#18559=CARTESIAN_POINT('',(2.725,2.4,-0.1));
#18560=CARTESIAN_POINT('Origin',(3.,2.4,1.2));
#18561=CARTESIAN_POINT('Origin',(21.,-7.8,-0.1));
#18562=CARTESIAN_POINT('',(20.79,-7.8,0.));
#18563=CARTESIAN_POINT('Origin',(21.,-7.8,0.));
#18564=CARTESIAN_POINT('',(20.79,-7.8,1.2));
#18565=CARTESIAN_POINT('',(20.79,-7.8,-0.1));
#18566=CARTESIAN_POINT('Origin',(21.,-7.8,1.2));
#18567=CARTESIAN_POINT('Origin',(1.,-4.2,-0.1));
#18568=CARTESIAN_POINT('',(0.79,-4.2,0.));
#18569=CARTESIAN_POINT('Origin',(1.,-4.2,0.));
#18570=CARTESIAN_POINT('',(0.79,-4.2,1.2));
#18571=CARTESIAN_POINT('',(0.79,-4.2,-0.1));
#18572=CARTESIAN_POINT('Origin',(1.,-4.2,1.2));
#18573=CARTESIAN_POINT('Origin',(1.,-7.8,-0.1));
#18574=CARTESIAN_POINT('',(0.79,-7.8,0.));
#18575=CARTESIAN_POINT('Origin',(1.,-7.8,0.));
#18576=CARTESIAN_POINT('',(0.79,-7.8,1.2));
#18577=CARTESIAN_POINT('',(0.79,-7.8,-0.1));
#18578=CARTESIAN_POINT('Origin',(1.,-7.8,1.2));
#18579=CARTESIAN_POINT('Origin',(21.,-4.2,-0.1));
#18580=CARTESIAN_POINT('',(20.79,-4.2,0.));
#18581=CARTESIAN_POINT('Origin',(21.,-4.2,0.));
#18582=CARTESIAN_POINT('',(20.79,-4.2,1.2));
#18583=CARTESIAN_POINT('',(20.79,-4.2,-0.1));
#18584=CARTESIAN_POINT('Origin',(21.,-4.2,1.2));
#18585=CARTESIAN_POINT('Origin',(27.,5.,0.));
#18586=CARTESIAN_POINT('',(27.,5.,0.));
#18587=CARTESIAN_POINT('',(0.,5.,0.));
#18588=CARTESIAN_POINT('',(27.,5.,0.));
#18589=CARTESIAN_POINT('',(0.,5.,1.2));
#18590=CARTESIAN_POINT('',(0.,5.,0.));
#18591=CARTESIAN_POINT('',(27.,5.,1.2));
#18592=CARTESIAN_POINT('',(27.,5.,1.2));
#18593=CARTESIAN_POINT('',(27.,5.,0.));
#18594=CARTESIAN_POINT('Origin',(27.,-10.,0.));
#18595=CARTESIAN_POINT('',(27.,-10.,0.));
#18596=CARTESIAN_POINT('',(27.,-10.,0.));
#18597=CARTESIAN_POINT('',(27.,-10.,1.2));
#18598=CARTESIAN_POINT('',(27.,-10.,1.2));
#18599=CARTESIAN_POINT('',(27.,-10.,0.));
#18600=CARTESIAN_POINT('Origin',(0.,-10.,0.));
#18601=CARTESIAN_POINT('',(0.,-10.,0.));
#18602=CARTESIAN_POINT('',(0.,-10.,0.));
#18603=CARTESIAN_POINT('',(0.,-10.,1.2));
#18604=CARTESIAN_POINT('',(0.,-10.,1.2));
#18605=CARTESIAN_POINT('',(0.,-10.,0.));
#18606=CARTESIAN_POINT('Origin',(0.,5.,0.));
#18607=CARTESIAN_POINT('',(0.,5.,0.));
#18608=CARTESIAN_POINT('',(0.,5.,1.2));
#18609=CARTESIAN_POINT('Origin',(13.5,-2.5,1.2));
#18610=CARTESIAN_POINT('Origin',(13.5,-2.5,0.));
#18611=CARTESIAN_POINT('',(0.,0.,0.));
#18612=CARTESIAN_POINT('Origin',(14.,-6.,1.1));
#18613=CARTESIAN_POINT('',(13.835,-6.,1.2));
#18614=CARTESIAN_POINT('Origin',(14.,-6.,1.2));
#18615=CARTESIAN_POINT('',(13.835,-6.,2.8));
#18616=CARTESIAN_POINT('',(13.835,-6.,1.1));
#18617=CARTESIAN_POINT('Origin',(14.,-6.,2.8));
#18618=CARTESIAN_POINT('Origin',(8.,-6.,1.1));
#18619=CARTESIAN_POINT('',(7.835,-6.,1.2));
#18620=CARTESIAN_POINT('Origin',(8.,-6.,1.2));
#18621=CARTESIAN_POINT('',(7.835,-6.,2.8));
#18622=CARTESIAN_POINT('',(7.835,-6.,1.1));
#18623=CARTESIAN_POINT('Origin',(8.,-6.,2.8));
#18624=CARTESIAN_POINT('Origin',(2.,-6.,1.1));
#18625=CARTESIAN_POINT('',(1.835,-6.,1.2));
#18626=CARTESIAN_POINT('Origin',(2.,-6.,1.2));
#18627=CARTESIAN_POINT('',(1.835,-6.,2.8));
#18628=CARTESIAN_POINT('',(1.835,-6.,1.1));
#18629=CARTESIAN_POINT('Origin',(2.,-6.,2.8));
#18630=CARTESIAN_POINT('Origin',(20.,-6.,1.1));
#18631=CARTESIAN_POINT('',(19.835,-6.,1.2));
#18632=CARTESIAN_POINT('Origin',(20.,-6.,1.2));
#18633=CARTESIAN_POINT('',(19.835,-6.,2.8));
#18634=CARTESIAN_POINT('',(19.835,-6.,1.1));
#18635=CARTESIAN_POINT('Origin',(20.,-6.,2.8));
#18636=CARTESIAN_POINT('Origin',(21.,-7.8,2.2));
#18637=CARTESIAN_POINT('',(20.5,-7.8,2.2));
#18638=CARTESIAN_POINT('Origin',(21.,-7.8,2.2));
#18639=CARTESIAN_POINT('',(20.5,-7.8,2.8));
#18640=CARTESIAN_POINT('',(20.5,-7.8,2.2));
#18641=CARTESIAN_POINT('Origin',(21.,-7.8,2.8));
#18642=CARTESIAN_POINT('Origin',(21.,-7.8,2.2));
#18643=CARTESIAN_POINT('',(20.725,-7.8,2.2));
#18644=CARTESIAN_POINT('Origin',(21.,-7.8,2.2));
#18645=CARTESIAN_POINT('Origin',(1.,-4.2,2.2));
#18646=CARTESIAN_POINT('',(0.5,-4.2,2.2));
#18647=CARTESIAN_POINT('Origin',(1.,-4.2,2.2));
#18648=CARTESIAN_POINT('',(0.5,-4.2,2.8));
#18649=CARTESIAN_POINT('',(0.5,-4.2,2.2));
#18650=CARTESIAN_POINT('Origin',(1.,-4.2,2.8));
#18651=CARTESIAN_POINT('Origin',(1.,-4.2,2.2));
#18652=CARTESIAN_POINT('',(0.725,-4.2,2.2));
#18653=CARTESIAN_POINT('Origin',(1.,-4.2,2.2));
#18654=CARTESIAN_POINT('Origin',(1.,-7.8,2.2));
#18655=CARTESIAN_POINT('',(0.5,-7.8,2.2));
#18656=CARTESIAN_POINT('Origin',(1.,-7.8,2.2));
#18657=CARTESIAN_POINT('',(0.5,-7.8,2.8));
#18658=CARTESIAN_POINT('',(0.5,-7.8,2.2));
#18659=CARTESIAN_POINT('Origin',(1.,-7.8,2.8));
#18660=CARTESIAN_POINT('Origin',(1.,-7.8,2.2));
#18661=CARTESIAN_POINT('',(0.725,-7.8,2.2));
#18662=CARTESIAN_POINT('Origin',(1.,-7.8,2.2));
#18663=CARTESIAN_POINT('Origin',(21.,-4.2,2.2));
#18664=CARTESIAN_POINT('',(20.5,-4.2,2.2));
#18665=CARTESIAN_POINT('Origin',(21.,-4.2,2.2));
#18666=CARTESIAN_POINT('',(20.5,-4.2,2.8));
#18667=CARTESIAN_POINT('',(20.5,-4.2,2.2));
#18668=CARTESIAN_POINT('Origin',(21.,-4.2,2.8));
#18669=CARTESIAN_POINT('Origin',(21.,-4.2,2.2));
#18670=CARTESIAN_POINT('',(20.725,-4.2,2.2));
#18671=CARTESIAN_POINT('Origin',(21.,-4.2,2.2));
#18672=CARTESIAN_POINT('Origin',(21.,-7.8,1.1));
#18673=CARTESIAN_POINT('',(20.725,-7.8,1.2));
#18674=CARTESIAN_POINT('Origin',(21.,-7.8,1.2));
#18675=CARTESIAN_POINT('',(20.725,-7.8,1.1));
#18676=CARTESIAN_POINT('Origin',(1.,-4.2,1.1));
#18677=CARTESIAN_POINT('',(0.725,-4.2,1.2));
#18678=CARTESIAN_POINT('Origin',(1.,-4.2,1.2));
#18679=CARTESIAN_POINT('',(0.725,-4.2,1.1));
#18680=CARTESIAN_POINT('Origin',(1.,-7.8,1.1));
#18681=CARTESIAN_POINT('',(0.725,-7.8,1.2));
#18682=CARTESIAN_POINT('Origin',(1.,-7.8,1.2));
#18683=CARTESIAN_POINT('',(0.725,-7.8,1.1));
#18684=CARTESIAN_POINT('Origin',(21.,-4.2,1.1));
#18685=CARTESIAN_POINT('',(20.725,-4.2,1.2));
#18686=CARTESIAN_POINT('Origin',(21.,-4.2,1.2));
#18687=CARTESIAN_POINT('',(20.725,-4.2,1.1));
#18688=CARTESIAN_POINT('Origin',(22.,-3.5,1.2));
#18689=CARTESIAN_POINT('',(22.,-3.5,1.2));
#18690=CARTESIAN_POINT('',(0.,-3.5,1.2));
#18691=CARTESIAN_POINT('',(22.,-3.5,1.2));
#18692=CARTESIAN_POINT('',(0.,-3.5,2.8));
#18693=CARTESIAN_POINT('',(0.,-3.5,1.2));
#18694=CARTESIAN_POINT('',(22.,-3.5,2.8));
#18695=CARTESIAN_POINT('',(22.,-3.5,2.8));
#18696=CARTESIAN_POINT('',(22.,-3.5,1.2));
#18697=CARTESIAN_POINT('Origin',(22.,-8.5,1.2));
#18698=CARTESIAN_POINT('',(22.,-8.5,1.2));
#18699=CARTESIAN_POINT('',(22.,-8.5,1.2));
#18700=CARTESIAN_POINT('',(22.,-8.5,2.8));
#18701=CARTESIAN_POINT('',(22.,-8.5,2.8));
#18702=CARTESIAN_POINT('',(22.,-8.5,1.2));
#18703=CARTESIAN_POINT('Origin',(0.,-8.5,1.2));
#18704=CARTESIAN_POINT('',(0.,-8.5,1.2));
#18705=CARTESIAN_POINT('',(0.,-8.5,1.2));
#18706=CARTESIAN_POINT('',(0.,-8.5,2.8));
#18707=CARTESIAN_POINT('',(0.,-8.5,2.8));
#18708=CARTESIAN_POINT('',(0.,-8.5,1.2));
#18709=CARTESIAN_POINT('Origin',(0.,-3.5,1.2));
#18710=CARTESIAN_POINT('',(0.,-3.5,1.2));
#18711=CARTESIAN_POINT('',(0.,-3.5,2.8));
#18712=CARTESIAN_POINT('Origin',(11.,-6.,2.8));
#18713=CARTESIAN_POINT('Origin',(11.,-6.,1.2));
#18714=CARTESIAN_POINT('',(0.,0.,0.));
#18715=CARTESIAN_POINT('Origin',(1.9,-2.1,4.));
#18716=CARTESIAN_POINT('',(2.,-2.1,4.165));
#18717=CARTESIAN_POINT('Origin',(2.,-2.1,4.));
#18718=CARTESIAN_POINT('',(4.,-2.1,4.165));
#18719=CARTESIAN_POINT('',(1.9,-2.1,4.165));
#18720=CARTESIAN_POINT('Origin',(4.,-2.1,4.));
#18721=CARTESIAN_POINT('Origin',(1.9,2.1,4.));
#18722=CARTESIAN_POINT('',(2.,2.1,4.165));
#18723=CARTESIAN_POINT('Origin',(2.,2.1,4.));
#18724=CARTESIAN_POINT('',(4.,2.1,4.165));
#18725=CARTESIAN_POINT('',(1.9,2.1,4.165));
#18726=CARTESIAN_POINT('Origin',(4.,2.1,4.));
#18727=CARTESIAN_POINT('Origin',(1.9,0.,6.1));
#18728=CARTESIAN_POINT('',(2.,-2.02066721859313E-17,6.265));
#18729=CARTESIAN_POINT('Origin',(2.,0.,6.1));
#18730=CARTESIAN_POINT('',(4.,2.02066721859313E-17,6.265));
#18731=CARTESIAN_POINT('',(1.9,-2.02066721859313E-17,6.265));
#18732=CARTESIAN_POINT('Origin',(4.,0.,6.1));
#18733=CARTESIAN_POINT('Origin',(1.9,0.,4.));
#18734=CARTESIAN_POINT('',(2.,-1.95943487863577E-16,5.6));
#18735=CARTESIAN_POINT('Origin',(2.,0.,4.));
#18736=CARTESIAN_POINT('',(3.5,-1.95943487863577E-16,5.6));
#18737=CARTESIAN_POINT('',(1.9,-1.95943487863577E-16,5.6));
#18738=CARTESIAN_POINT('Origin',(3.5,0.,4.));
#18739=CARTESIAN_POINT('Origin',(3.5,0.,4.));
#18740=CARTESIAN_POINT('',(3.5,1.71450551880629E-16,5.4));
#18741=CARTESIAN_POINT('Origin',(3.5,0.,4.));
#18742=CARTESIAN_POINT('Origin',(1.9,0.,4.));
#18743=CARTESIAN_POINT('',(4.,1.71450551880629E-16,5.4));
#18744=CARTESIAN_POINT('',(1.9,-1.71450551880629E-16,5.4));
#18745=CARTESIAN_POINT('Origin',(4.,0.,4.));
#18746=CARTESIAN_POINT('Origin',(3.,-2.4,1.1));
#18747=CARTESIAN_POINT('',(2.79,-2.4,1.2));
#18748=CARTESIAN_POINT('Origin',(3.,-2.4,1.2));
#18749=CARTESIAN_POINT('',(2.79,-2.4,2.9));
#18750=CARTESIAN_POINT('',(2.79,-2.4,1.1));
#18751=CARTESIAN_POINT('Origin',(3.,-2.4,2.9));
#18752=CARTESIAN_POINT('Origin',(3.,-2.4,2.9));
#18753=CARTESIAN_POINT('Origin',(3.,2.4,1.1));
#18754=CARTESIAN_POINT('',(2.79,2.4,1.2));
#18755=CARTESIAN_POINT('Origin',(3.,2.4,1.2));
#18756=CARTESIAN_POINT('',(2.79,2.4,2.9));
#18757=CARTESIAN_POINT('',(2.79,2.4,1.1));
#18758=CARTESIAN_POINT('Origin',(3.,2.4,2.9));
#18759=CARTESIAN_POINT('Origin',(3.,2.4,2.9));
#18760=CARTESIAN_POINT('Origin',(4.,3.,1.2));
#18761=CARTESIAN_POINT('',(4.,3.,1.2));
#18762=CARTESIAN_POINT('',(2.,3.,1.2));
#18763=CARTESIAN_POINT('',(4.,3.,1.2));
#18764=CARTESIAN_POINT('',(2.,3.,7.));
#18765=CARTESIAN_POINT('',(2.,3.,1.2));
#18766=CARTESIAN_POINT('',(4.,3.,7.));
#18767=CARTESIAN_POINT('',(4.,3.,7.));
#18768=CARTESIAN_POINT('',(4.,3.,1.2));
#18769=CARTESIAN_POINT('Origin',(4.,-3.,1.2));
#18770=CARTESIAN_POINT('',(4.,-3.,1.2));
#18771=CARTESIAN_POINT('',(4.,-3.,1.2));
#18772=CARTESIAN_POINT('',(4.,-3.,7.));
#18773=CARTESIAN_POINT('',(4.,-3.,7.));
#18774=CARTESIAN_POINT('',(4.,-3.,1.2));
#18775=CARTESIAN_POINT('Origin',(2.,-3.,1.2));
#18776=CARTESIAN_POINT('',(2.,-3.,1.2));
#18777=CARTESIAN_POINT('',(2.,-3.,1.2));
#18778=CARTESIAN_POINT('',(2.,-3.,7.));
#18779=CARTESIAN_POINT('',(2.,-3.,7.));
#18780=CARTESIAN_POINT('',(2.,-3.,1.2));
#18781=CARTESIAN_POINT('Origin',(2.,3.,1.2));
#18782=CARTESIAN_POINT('',(2.,3.,1.2));
#18783=CARTESIAN_POINT('',(2.,3.,7.));
#18784=CARTESIAN_POINT('Origin',(3.,0.,7.));
#18785=CARTESIAN_POINT('Origin',(3.,0.,1.2));
#18786=CARTESIAN_POINT('',(0.,0.,0.));
#18787=CARTESIAN_POINT('Origin',(1.5,-2.1,4.));
#18788=CARTESIAN_POINT('',(1.6,-2.1,4.225));
#18789=CARTESIAN_POINT('Origin',(1.6,-2.1,4.));
#18790=CARTESIAN_POINT('',(2.,-2.1,4.225));
#18791=CARTESIAN_POINT('',(1.5,-2.1,4.225));
#18792=CARTESIAN_POINT('Origin',(2.,-2.1,4.));
#18793=CARTESIAN_POINT('Origin',(1.5,2.1,4.));
#18794=CARTESIAN_POINT('',(1.6,2.1,4.225));
#18795=CARTESIAN_POINT('Origin',(1.6,2.1,4.));
#18796=CARTESIAN_POINT('',(2.,2.1,4.225));
#18797=CARTESIAN_POINT('',(1.5,2.1,4.225));
#18798=CARTESIAN_POINT('Origin',(2.,2.1,4.));
#18799=CARTESIAN_POINT('Origin',(1.5,0.,6.1));
#18800=CARTESIAN_POINT('',(1.6,-2.75545529808154E-17,6.325));
#18801=CARTESIAN_POINT('Origin',(1.6,0.,6.1));
#18802=CARTESIAN_POINT('',(2.,2.75545529808154E-17,6.325));
#18803=CARTESIAN_POINT('',(1.5,-2.75545529808154E-17,6.325));
#18804=CARTESIAN_POINT('Origin',(2.,0.,6.1));
#18805=CARTESIAN_POINT('Origin',(2.,0.,4.));
#18806=CARTESIAN_POINT('',(2.5,-1.94718841064429E-16,5.59));
#18807=CARTESIAN_POINT('Origin',(2.5,0.,4.));
#18808=CARTESIAN_POINT('',(2.,-1.94718841064429E-16,5.59));
#18809=CARTESIAN_POINT('',(2.,-1.94718841064429E-16,5.59));
#18810=CARTESIAN_POINT('Origin',(2.,0.,4.));
#18811=CARTESIAN_POINT('Origin',(2.5,0.,4.));
#18812=CARTESIAN_POINT('',(2.5,-1.46957615897682E-16,5.2));
#18813=CARTESIAN_POINT('Origin',(2.5,0.,4.));
#18814=CARTESIAN_POINT('Origin',(1.6,0.,4.));
#18815=CARTESIAN_POINT('',(1.6,-1.46957615897682E-16,5.2));
#18816=CARTESIAN_POINT('',(1.6,-1.46957615897682E-16,5.2));
#18817=CARTESIAN_POINT('Origin',(1.6,0.,4.));
#18818=CARTESIAN_POINT('Origin',(1.6,0.,4.));
#18819=CARTESIAN_POINT('',(2.,-2.93915231795365E-16,6.4));
#18820=CARTESIAN_POINT('Origin',(2.,0.,4.));
#18821=CARTESIAN_POINT('',(1.6,-2.93915231795365E-16,6.4));
#18822=CARTESIAN_POINT('',(1.6,-2.93915231795365E-16,6.4));
#18823=CARTESIAN_POINT('Origin',(1.6,0.,4.));
#18824=CARTESIAN_POINT('Origin',(2.,0.,4.));
#18825=CARTESIAN_POINT('Origin',(1.6,0.,4.));
#18826=CARTESIAN_POINT('',(0.,0.,0.));
#18827=CARTESIAN_POINT('Origin',(22.9,-2.6,4.));
#18828=CARTESIAN_POINT('',(23.,-2.6,4.165));
#18829=CARTESIAN_POINT('Origin',(23.,-2.6,4.));
#18830=CARTESIAN_POINT('',(25.,-2.6,4.165));
#18831=CARTESIAN_POINT('',(22.9,-2.6,4.165));
#18832=CARTESIAN_POINT('Origin',(25.,-2.6,4.));
#18833=CARTESIAN_POINT('Origin',(22.9,2.6,4.));
#18834=CARTESIAN_POINT('',(23.,2.6,4.165));
#18835=CARTESIAN_POINT('Origin',(23.,2.6,4.));
#18836=CARTESIAN_POINT('',(25.,2.6,4.165));
#18837=CARTESIAN_POINT('',(22.9,2.6,4.165));
#18838=CARTESIAN_POINT('Origin',(25.,2.6,4.));
#18839=CARTESIAN_POINT('Origin',(22.9,0.,6.6));
#18840=CARTESIAN_POINT('',(23.,-2.02066721859313E-17,6.765));
#18841=CARTESIAN_POINT('Origin',(23.,0.,6.6));
#18842=CARTESIAN_POINT('',(25.,2.02066721859313E-17,6.765));
#18843=CARTESIAN_POINT('',(22.9,-2.02066721859313E-17,6.765));
#18844=CARTESIAN_POINT('Origin',(25.,0.,6.6));
#18845=CARTESIAN_POINT('Origin',(23.3,0.,4.));
#18846=CARTESIAN_POINT('',(23.3,-2.87791997799628E-16,6.35));
#18847=CARTESIAN_POINT('Origin',(23.3,0.,4.));
#18848=CARTESIAN_POINT('',(25.,2.87791997799628E-16,6.35));
#18849=CARTESIAN_POINT('',(23.3,-2.87791997799628E-16,6.35));
#18850=CARTESIAN_POINT('Origin',(25.,0.,4.));
#18851=CARTESIAN_POINT('Origin',(23.3,0.,4.));
#18852=CARTESIAN_POINT('',(23.3,-2.63299061816681E-16,6.15));
#18853=CARTESIAN_POINT('Origin',(23.3,0.,4.));
#18854=CARTESIAN_POINT('Origin',(22.9,0.,4.));
#18855=CARTESIAN_POINT('',(23.,-2.63299061816681E-16,6.15));
#18856=CARTESIAN_POINT('Origin',(23.,0.,4.));
#18857=CARTESIAN_POINT('',(22.9,-2.63299061816681E-16,6.15));
#18858=CARTESIAN_POINT('Origin',(24.,-3.5,1.1));
#18859=CARTESIAN_POINT('',(23.75,-3.5,1.2));
#18860=CARTESIAN_POINT('Origin',(24.,-3.5,1.2));
#18861=CARTESIAN_POINT('',(23.75,-3.5,2.9));
#18862=CARTESIAN_POINT('',(23.75,-3.5,1.1));
#18863=CARTESIAN_POINT('Origin',(24.,-3.5,2.9));
#18864=CARTESIAN_POINT('Origin',(24.,-3.5,2.9));
#18865=CARTESIAN_POINT('Origin',(24.,3.5,1.1));
#18866=CARTESIAN_POINT('',(23.75,3.5,1.2));
#18867=CARTESIAN_POINT('Origin',(24.,3.5,1.2));
#18868=CARTESIAN_POINT('',(23.75,3.5,2.9));
#18869=CARTESIAN_POINT('',(23.75,3.5,1.1));
#18870=CARTESIAN_POINT('Origin',(24.,3.5,2.9));
#18871=CARTESIAN_POINT('Origin',(24.,3.5,2.9));
#18872=CARTESIAN_POINT('Origin',(25.,5.,1.2));
#18873=CARTESIAN_POINT('',(25.,5.,1.2));
#18874=CARTESIAN_POINT('',(23.,5.,1.2));
#18875=CARTESIAN_POINT('',(25.,5.,1.2));
#18876=CARTESIAN_POINT('',(23.,5.,7.));
#18877=CARTESIAN_POINT('',(23.,5.,1.2));
#18878=CARTESIAN_POINT('',(25.,5.,7.));
#18879=CARTESIAN_POINT('',(25.,5.,7.));
#18880=CARTESIAN_POINT('',(25.,5.,1.2));
#18881=CARTESIAN_POINT('Origin',(25.,-5.,1.2));
#18882=CARTESIAN_POINT('',(25.,-5.,1.2));
#18883=CARTESIAN_POINT('',(25.,-5.,1.2));
#18884=CARTESIAN_POINT('',(25.,-5.,7.));
#18885=CARTESIAN_POINT('',(25.,-5.,7.));
#18886=CARTESIAN_POINT('',(25.,-5.,1.2));
#18887=CARTESIAN_POINT('Origin',(23.,-5.,1.2));
#18888=CARTESIAN_POINT('',(23.,-5.,1.2));
#18889=CARTESIAN_POINT('',(23.,-5.,1.2));
#18890=CARTESIAN_POINT('',(23.,-5.,7.));
#18891=CARTESIAN_POINT('',(23.,-5.,7.));
#18892=CARTESIAN_POINT('',(23.,-5.,1.2));
#18893=CARTESIAN_POINT('Origin',(23.,5.,1.2));
#18894=CARTESIAN_POINT('',(23.,5.,1.2));
#18895=CARTESIAN_POINT('',(23.,5.,7.));
#18896=CARTESIAN_POINT('Origin',(24.,0.,7.));
#18897=CARTESIAN_POINT('Origin',(24.,0.,1.2));
#18898=CARTESIAN_POINT('',(0.,0.,0.));
#18899=CARTESIAN_POINT('Origin',(24.9,3.5,1.22));
#18900=CARTESIAN_POINT('',(25.,-1.12765242872084,1.22));
#18901=CARTESIAN_POINT('',(25.4,-1.12765242872084,1.22));
#18902=CARTESIAN_POINT('',(25.,-1.12765242872084,1.22));
#18903=CARTESIAN_POINT('',(25.,1.12765242872084,1.22));
#18904=CARTESIAN_POINT('',(25.,1.75,1.22));
#18905=CARTESIAN_POINT('',(25.4,1.12765242872084,1.22));
#18906=CARTESIAN_POINT('',(25.,1.12765242872084,1.22));
#18907=CARTESIAN_POINT('',(25.4,1.75,1.22));
#18908=CARTESIAN_POINT('Origin',(25.,0.,4.));
#18909=CARTESIAN_POINT('Origin',(25.,0.,4.));
#18910=CARTESIAN_POINT('',(25.,-2.86567351000481E-16,6.34));
#18911=CARTESIAN_POINT('Origin',(25.,0.,4.));
#18912=CARTESIAN_POINT('',(25.,-2.75545529808154E-17,6.825));
#18913=CARTESIAN_POINT('Origin',(25.,0.,6.6));
#18914=CARTESIAN_POINT('',(25.,2.6,4.225));
#18915=CARTESIAN_POINT('Origin',(25.,2.6,4.));
#18916=CARTESIAN_POINT('',(25.,-2.6,4.225));
#18917=CARTESIAN_POINT('Origin',(25.,-2.6,4.));
#18918=CARTESIAN_POINT('Origin',(25.,0.,4.));
#18919=CARTESIAN_POINT('Origin',(25.4,0.,4.));
#18920=CARTESIAN_POINT('Origin',(24.9,-2.6,4.));
#18921=CARTESIAN_POINT('',(25.4,-2.6,4.225));
#18922=CARTESIAN_POINT('',(24.9,-2.6,4.225));
#18923=CARTESIAN_POINT('Origin',(25.4,-2.6,4.));
#18924=CARTESIAN_POINT('Origin',(24.9,2.6,4.));
#18925=CARTESIAN_POINT('',(25.4,2.6,4.225));
#18926=CARTESIAN_POINT('',(24.9,2.6,4.225));
#18927=CARTESIAN_POINT('Origin',(25.4,2.6,4.));
#18928=CARTESIAN_POINT('Origin',(24.9,0.,6.6));
#18929=CARTESIAN_POINT('',(25.4,2.75545529808154E-17,6.825));
#18930=CARTESIAN_POINT('',(24.9,-2.75545529808154E-17,6.825));
#18931=CARTESIAN_POINT('Origin',(25.4,0.,6.6));
#18932=CARTESIAN_POINT('Origin',(24.7,0.,4.));
#18933=CARTESIAN_POINT('',(24.7,-2.86567351000481E-16,6.34));
#18934=CARTESIAN_POINT('',(24.7,-2.86567351000481E-16,6.34));
#18935=CARTESIAN_POINT('Origin',(24.7,0.,4.));
#18936=CARTESIAN_POINT('Origin',(24.7,0.,4.));
#18937=CARTESIAN_POINT('',(24.7,-2.20436423846524E-16,5.8));
#18938=CARTESIAN_POINT('Origin',(24.7,0.,4.));
#18939=CARTESIAN_POINT('Origin',(25.,0.,4.));
#18940=CARTESIAN_POINT('',(25.4,-2.20436423846524E-16,5.8));
#18941=CARTESIAN_POINT('Origin',(25.4,0.,4.));
#18942=CARTESIAN_POINT('',(25.,-2.20436423846524E-16,5.8));
#18943=CARTESIAN_POINT('Origin',(25.4,0.,4.));
#18944=CARTESIAN_POINT('',(0.,0.,0.));
#18945=CARTESIAN_POINT('Origin',(4.7,-9.,2.4));
#18946=CARTESIAN_POINT('',(4.44382623085101,-8.6,2.4));
#18947=CARTESIAN_POINT('',(4.95617376914899,-8.6,2.4));
#18948=CARTESIAN_POINT('',(4.4,-8.6,2.4));
#18949=CARTESIAN_POINT('',(4.225,-9.,2.4));
#18950=CARTESIAN_POINT('Origin',(4.7,-9.,2.4));
#18951=CARTESIAN_POINT('Origin',(4.7,-9.,2.4));
#18952=CARTESIAN_POINT('',(4.425,-9.,2.4));
#18953=CARTESIAN_POINT('Origin',(4.7,-9.,2.4));
#18954=CARTESIAN_POINT('Origin',(4.7,-9.,2.4));
#18955=CARTESIAN_POINT('',(4.44382623085101,-8.6,5.2));
#18956=CARTESIAN_POINT('',(4.44382623085101,-8.6,2.4));
#18957=CARTESIAN_POINT('',(4.95617376914899,-8.6,5.2));
#18958=CARTESIAN_POINT('Origin',(4.7,-9.,5.2));
#18959=CARTESIAN_POINT('',(4.95617376914899,-8.6,2.4));
#18960=CARTESIAN_POINT('',(4.225,-9.,7.));
#18961=CARTESIAN_POINT('',(4.225,-9.,2.4));
#18962=CARTESIAN_POINT('Origin',(4.7,-9.,7.));
#18963=CARTESIAN_POINT('Origin',(4.7,-3.,2.4));
#18964=CARTESIAN_POINT('',(4.95617376914899,-3.4,2.4));
#18965=CARTESIAN_POINT('',(4.44382623085101,-3.4,2.4));
#18966=CARTESIAN_POINT('',(4.4,-3.4,2.4));
#18967=CARTESIAN_POINT('',(4.225,-3.,2.4));
#18968=CARTESIAN_POINT('Origin',(4.7,-3.,2.4));
#18969=CARTESIAN_POINT('Origin',(4.7,-3.,2.4));
#18970=CARTESIAN_POINT('',(4.425,-3.,2.4));
#18971=CARTESIAN_POINT('Origin',(4.7,-3.,2.4));
#18972=CARTESIAN_POINT('Origin',(4.7,-3.,2.4));
#18973=CARTESIAN_POINT('',(4.95617376914899,-3.4,5.2));
#18974=CARTESIAN_POINT('',(4.95617376914899,-3.4,2.4));
#18975=CARTESIAN_POINT('',(4.44382623085101,-3.4,5.2));
#18976=CARTESIAN_POINT('Origin',(4.7,-3.,5.2));
#18977=CARTESIAN_POINT('',(4.44382623085101,-3.4,2.4));
#18978=CARTESIAN_POINT('',(4.225,-3.,7.));
#18979=CARTESIAN_POINT('',(4.225,-3.,2.4));
#18980=CARTESIAN_POINT('Origin',(4.7,-3.,7.));
#18981=CARTESIAN_POINT('Origin',(4.1,-8.6,5.2));
#18982=CARTESIAN_POINT('',(5.2,-8.6,5.2));
#18983=CARTESIAN_POINT('',(4.1,-8.6,5.2));
#18984=CARTESIAN_POINT('',(5.2,-8.6,1.2));
#18985=CARTESIAN_POINT('',(5.2,-8.6,3.2));
#18986=CARTESIAN_POINT('',(4.2,-8.6,1.2));
#18987=CARTESIAN_POINT('',(4.4,-8.6,1.2));
#18988=CARTESIAN_POINT('',(4.2,-8.6,5.2));
#18989=CARTESIAN_POINT('',(4.2,-8.6,3.2));
#18990=CARTESIAN_POINT('',(4.1,-8.6,5.2));
#18991=CARTESIAN_POINT('Origin',(4.1,-3.4,1.2));
#18992=CARTESIAN_POINT('',(4.2,-3.4,5.2));
#18993=CARTESIAN_POINT('',(4.1,-3.4,5.2));
#18994=CARTESIAN_POINT('',(4.2,-3.4,1.2));
#18995=CARTESIAN_POINT('',(4.2,-3.4,1.2));
#18996=CARTESIAN_POINT('',(5.2,-3.4,1.2));
#18997=CARTESIAN_POINT('',(4.4,-3.4,1.2));
#18998=CARTESIAN_POINT('',(5.2,-3.4,5.2));
#18999=CARTESIAN_POINT('',(5.2,-3.4,1.2));
#19000=CARTESIAN_POINT('',(4.1,-3.4,5.2));
#19001=CARTESIAN_POINT('Origin',(4.7,-9.,1.1));
#19002=CARTESIAN_POINT('',(4.425,-9.,1.2));
#19003=CARTESIAN_POINT('Origin',(4.7,-9.,1.2));
#19004=CARTESIAN_POINT('',(4.425,-9.,1.1));
#19005=CARTESIAN_POINT('Origin',(4.7,-3.,1.1));
#19006=CARTESIAN_POINT('',(4.425,-3.,1.2));
#19007=CARTESIAN_POINT('Origin',(4.7,-3.,1.2));
#19008=CARTESIAN_POINT('',(4.425,-3.,1.1));
#19009=CARTESIAN_POINT('Origin',(4.1,-3.4,5.2));
#19010=CARTESIAN_POINT('',(4.2,-2.95,5.2));
#19011=CARTESIAN_POINT('',(5.2,-6.45,5.2));
#19012=CARTESIAN_POINT('Origin',(5.2,-9.5,1.2));
#19013=CARTESIAN_POINT('',(5.2,-2.5,1.2));
#19014=CARTESIAN_POINT('',(5.2,-9.5,1.2));
#19015=CARTESIAN_POINT('',(5.2,-2.5,7.));
#19016=CARTESIAN_POINT('',(5.2,-2.5,1.2));
#19017=CARTESIAN_POINT('',(5.2,-9.5,7.));
#19018=CARTESIAN_POINT('',(5.2,-9.5,7.));
#19019=CARTESIAN_POINT('',(5.2,-9.5,1.2));
#19020=CARTESIAN_POINT('',(5.2,-9.5,1.2));
#19021=CARTESIAN_POINT('',(5.2,-9.5,1.2));
#19022=CARTESIAN_POINT('Origin',(4.7,-6.,1.2));
#19023=CARTESIAN_POINT('',(4.2,-2.5,1.2));
#19024=CARTESIAN_POINT('',(4.2,-2.5,1.2));
#19025=CARTESIAN_POINT('',(5.2,-2.5,1.2));
#19026=CARTESIAN_POINT('Origin',(5.2,-2.5,1.2));
#19027=CARTESIAN_POINT('',(4.2,-2.5,7.));
#19028=CARTESIAN_POINT('',(4.2,-2.5,1.2));
#19029=CARTESIAN_POINT('',(5.2,-2.5,7.));
#19030=CARTESIAN_POINT('Origin',(4.2,-9.5,1.2));
#19031=CARTESIAN_POINT('',(4.2,-9.5,1.2));
#19032=CARTESIAN_POINT('',(4.2,-9.5,1.2));
#19033=CARTESIAN_POINT('',(4.2,-9.5,7.));
#19034=CARTESIAN_POINT('',(4.2,-9.5,7.));
#19035=CARTESIAN_POINT('',(4.2,-9.5,1.2));
#19036=CARTESIAN_POINT('Origin',(4.2,-2.5,1.2));
#19037=CARTESIAN_POINT('',(4.2,-2.5,1.2));
#19038=CARTESIAN_POINT('',(4.2,-2.5,7.));
#19039=CARTESIAN_POINT('Origin',(4.7,-6.,7.));
#19040=CARTESIAN_POINT('Origin',(4.7,-6.,1.2));
#19041=CARTESIAN_POINT('',(0.,0.,0.));
#19042=CARTESIAN_POINT('Origin',(22.3,-9.,2.4));
#19043=CARTESIAN_POINT('',(22.043826230851,-8.6,2.4));
#19044=CARTESIAN_POINT('',(22.556173769149,-8.6,2.4));
#19045=CARTESIAN_POINT('',(22.,-8.6,2.4));
#19046=CARTESIAN_POINT('',(21.825,-9.,2.4));
#19047=CARTESIAN_POINT('Origin',(22.3,-9.,2.4));
#19048=CARTESIAN_POINT('Origin',(22.3,-9.,2.4));
#19049=CARTESIAN_POINT('',(22.025,-9.,2.4));
#19050=CARTESIAN_POINT('Origin',(22.3,-9.,2.4));
#19051=CARTESIAN_POINT('Origin',(22.3,-9.,2.4));
#19052=CARTESIAN_POINT('',(22.043826230851,-8.6,5.2));
#19053=CARTESIAN_POINT('',(22.043826230851,-8.6,2.4));
#19054=CARTESIAN_POINT('',(22.556173769149,-8.6,5.2));
#19055=CARTESIAN_POINT('Origin',(22.3,-9.,5.2));
#19056=CARTESIAN_POINT('',(22.556173769149,-8.6,2.4));
#19057=CARTESIAN_POINT('',(21.825,-9.,7.));
#19058=CARTESIAN_POINT('',(21.825,-9.,2.4));
#19059=CARTESIAN_POINT('Origin',(22.3,-9.,7.));
#19060=CARTESIAN_POINT('Origin',(22.3,-3.,2.4));
#19061=CARTESIAN_POINT('',(22.556173769149,-3.4,2.4));
#19062=CARTESIAN_POINT('',(22.043826230851,-3.4,2.4));
#19063=CARTESIAN_POINT('',(22.,-3.4,2.4));
#19064=CARTESIAN_POINT('',(21.825,-3.,2.4));
#19065=CARTESIAN_POINT('Origin',(22.3,-3.,2.4));
#19066=CARTESIAN_POINT('Origin',(22.3,-3.,2.4));
#19067=CARTESIAN_POINT('',(22.025,-3.,2.4));
#19068=CARTESIAN_POINT('Origin',(22.3,-3.,2.4));
#19069=CARTESIAN_POINT('Origin',(22.3,-3.,2.4));
#19070=CARTESIAN_POINT('',(22.556173769149,-3.4,5.2));
#19071=CARTESIAN_POINT('',(22.556173769149,-3.4,2.4));
#19072=CARTESIAN_POINT('',(22.043826230851,-3.4,5.2));
#19073=CARTESIAN_POINT('Origin',(22.3,-3.,5.2));
#19074=CARTESIAN_POINT('',(22.043826230851,-3.4,2.4));
#19075=CARTESIAN_POINT('',(21.825,-3.,7.));
#19076=CARTESIAN_POINT('',(21.825,-3.,2.4));
#19077=CARTESIAN_POINT('Origin',(22.3,-3.,7.));
#19078=CARTESIAN_POINT('Origin',(21.7,-8.6,5.2));
#19079=CARTESIAN_POINT('',(22.8,-8.6,5.2));
#19080=CARTESIAN_POINT('',(21.7,-8.6,5.2));
#19081=CARTESIAN_POINT('',(22.8,-8.6,1.2));
#19082=CARTESIAN_POINT('',(22.8,-8.6,3.2));
#19083=CARTESIAN_POINT('',(21.8,-8.6,1.2));
#19084=CARTESIAN_POINT('',(22.,-8.6,1.2));
#19085=CARTESIAN_POINT('',(21.8,-8.6,5.2));
#19086=CARTESIAN_POINT('',(21.8,-8.6,3.2));
#19087=CARTESIAN_POINT('',(21.7,-8.6,5.2));
#19088=CARTESIAN_POINT('Origin',(21.7,-3.4,1.2));
#19089=CARTESIAN_POINT('',(21.8,-3.4,5.2));
#19090=CARTESIAN_POINT('',(21.7,-3.4,5.2));
#19091=CARTESIAN_POINT('',(21.8,-3.4,1.2));
#19092=CARTESIAN_POINT('',(21.8,-3.4,1.2));
#19093=CARTESIAN_POINT('',(22.8,-3.4,1.2));
#19094=CARTESIAN_POINT('',(22.,-3.4,1.2));
#19095=CARTESIAN_POINT('',(22.8,-3.4,5.2));
#19096=CARTESIAN_POINT('',(22.8,-3.4,1.2));
#19097=CARTESIAN_POINT('',(21.7,-3.4,5.2));
#19098=CARTESIAN_POINT('Origin',(22.3,-9.,1.1));
#19099=CARTESIAN_POINT('',(22.025,-9.,1.2));
#19100=CARTESIAN_POINT('Origin',(22.3,-9.,1.2));
#19101=CARTESIAN_POINT('',(22.025,-9.,1.1));
#19102=CARTESIAN_POINT('Origin',(22.3,-3.,1.1));
#19103=CARTESIAN_POINT('',(22.025,-3.,1.2));
#19104=CARTESIAN_POINT('Origin',(22.3,-3.,1.2));
#19105=CARTESIAN_POINT('',(22.025,-3.,1.1));
#19106=CARTESIAN_POINT('Origin',(21.7,-3.4,5.2));
#19107=CARTESIAN_POINT('',(21.8,-2.95,5.2));
#19108=CARTESIAN_POINT('',(22.8,-6.45,5.2));
#19109=CARTESIAN_POINT('Origin',(22.8,-9.5,1.2));
#19110=CARTESIAN_POINT('',(22.8,-2.5,1.2));
#19111=CARTESIAN_POINT('',(22.8,-9.5,1.2));
#19112=CARTESIAN_POINT('',(22.8,-2.5,7.));
#19113=CARTESIAN_POINT('',(22.8,-2.5,1.2));
#19114=CARTESIAN_POINT('',(22.8,-9.5,7.));
#19115=CARTESIAN_POINT('',(22.8,-9.5,7.));
#19116=CARTESIAN_POINT('',(22.8,-9.5,1.2));
#19117=CARTESIAN_POINT('',(22.8,-9.5,1.2));
#19118=CARTESIAN_POINT('',(22.8,-9.5,1.2));
#19119=CARTESIAN_POINT('Origin',(22.3,-6.,1.2));
#19120=CARTESIAN_POINT('',(21.8,-2.5,1.2));
#19121=CARTESIAN_POINT('',(21.8,-2.5,1.2));
#19122=CARTESIAN_POINT('',(22.8,-2.5,1.2));
#19123=CARTESIAN_POINT('Origin',(22.8,-2.5,1.2));
#19124=CARTESIAN_POINT('',(21.8,-2.5,7.));
#19125=CARTESIAN_POINT('',(21.8,-2.5,1.2));
#19126=CARTESIAN_POINT('',(22.8,-2.5,7.));
#19127=CARTESIAN_POINT('Origin',(21.8,-9.5,1.2));
#19128=CARTESIAN_POINT('',(21.8,-9.5,1.2));
#19129=CARTESIAN_POINT('',(21.8,-9.5,1.2));
#19130=CARTESIAN_POINT('',(21.8,-9.5,7.));
#19131=CARTESIAN_POINT('',(21.8,-9.5,7.));
#19132=CARTESIAN_POINT('',(21.8,-9.5,1.2));
#19133=CARTESIAN_POINT('Origin',(21.8,-2.5,1.2));
#19134=CARTESIAN_POINT('',(21.8,-2.5,1.2));
#19135=CARTESIAN_POINT('',(21.8,-2.5,7.));
#19136=CARTESIAN_POINT('Origin',(22.3,-6.,7.));
#19137=CARTESIAN_POINT('Origin',(22.3,-6.,1.2));
#19138=CARTESIAN_POINT('',(0.,0.,0.));
#19139=CARTESIAN_POINT('Origin',(14.,0.,0.97));
#19140=CARTESIAN_POINT('',(13.625,-4.59242549680257E-17,0.97));
#19141=CARTESIAN_POINT('Origin',(14.,0.,0.97));
#19142=CARTESIAN_POINT('',(13.625,4.59242549680257E-17,1.5));
#19143=CARTESIAN_POINT('',(13.625,-4.59242549680257E-17,0.97));
#19144=CARTESIAN_POINT('Origin',(14.,0.,1.5));
#19145=CARTESIAN_POINT('Origin',(14.,0.,0.97));
#19146=CARTESIAN_POINT('',(13.775,-2.75545529808154E-17,0.97));
#19147=CARTESIAN_POINT('Origin',(14.,0.,0.97));
#19148=CARTESIAN_POINT('Origin',(8.,0.,0.97));
#19149=CARTESIAN_POINT('',(7.625,-4.59242549680257E-17,0.97));
#19150=CARTESIAN_POINT('Origin',(8.,0.,0.97));
#19151=CARTESIAN_POINT('',(7.625,4.59242549680257E-17,1.5));
#19152=CARTESIAN_POINT('',(7.625,-4.59242549680257E-17,0.97));
#19153=CARTESIAN_POINT('Origin',(8.,0.,1.5));
#19154=CARTESIAN_POINT('Origin',(8.,0.,0.97));
#19155=CARTESIAN_POINT('',(7.775,-2.75545529808154E-17,0.97));
#19156=CARTESIAN_POINT('Origin',(8.,0.,0.97));
#19157=CARTESIAN_POINT('Origin',(2.,0.,0.97));
#19158=CARTESIAN_POINT('',(1.625,-4.59242549680257E-17,0.97));
#19159=CARTESIAN_POINT('Origin',(2.,0.,0.97));
#19160=CARTESIAN_POINT('',(1.625,4.59242549680257E-17,1.5));
#19161=CARTESIAN_POINT('',(1.625,-4.59242549680257E-17,0.97));
#19162=CARTESIAN_POINT('Origin',(2.,0.,1.5));
#19163=CARTESIAN_POINT('Origin',(2.,0.,0.97));
#19164=CARTESIAN_POINT('',(1.775,-2.75545529808155E-17,0.97));
#19165=CARTESIAN_POINT('Origin',(2.,0.,0.97));
#19166=CARTESIAN_POINT('Origin',(20.,0.,0.97));
#19167=CARTESIAN_POINT('',(19.625,-4.59242549680257E-17,0.97));
#19168=CARTESIAN_POINT('Origin',(20.,0.,0.97));
#19169=CARTESIAN_POINT('',(19.625,4.59242549680257E-17,1.5));
#19170=CARTESIAN_POINT('',(19.625,-4.59242549680257E-17,0.97));
#19171=CARTESIAN_POINT('Origin',(20.,0.,1.5));
#19172=CARTESIAN_POINT('Origin',(20.,0.,0.97));
#19173=CARTESIAN_POINT('',(19.775,-2.75545529808156E-17,0.97));
#19174=CARTESIAN_POINT('Origin',(20.,0.,0.97));
#19175=CARTESIAN_POINT('Origin',(14.,0.,-0.1));
#19176=CARTESIAN_POINT('',(13.775,-2.75545529808154E-17,0.));
#19177=CARTESIAN_POINT('Origin',(14.,0.,0.));
#19178=CARTESIAN_POINT('',(13.775,-2.75545529808154E-17,-0.1));
#19179=CARTESIAN_POINT('Origin',(8.,0.,-0.1));
#19180=CARTESIAN_POINT('',(7.775,-2.75545529808154E-17,0.));
#19181=CARTESIAN_POINT('Origin',(8.,0.,0.));
#19182=CARTESIAN_POINT('',(7.775,-2.75545529808154E-17,-0.1));
#19183=CARTESIAN_POINT('Origin',(2.,0.,-0.1));
#19184=CARTESIAN_POINT('',(1.775,-2.75545529808155E-17,0.));
#19185=CARTESIAN_POINT('Origin',(2.,0.,0.));
#19186=CARTESIAN_POINT('',(1.775,-2.75545529808155E-17,-0.1));
#19187=CARTESIAN_POINT('Origin',(20.,0.,-0.1));
#19188=CARTESIAN_POINT('',(19.775,-2.75545529808156E-17,0.));
#19189=CARTESIAN_POINT('Origin',(20.,0.,0.));
#19190=CARTESIAN_POINT('',(19.775,-2.75545529808156E-17,-0.1));
#19191=CARTESIAN_POINT('Origin',(0.,-0.53,1.));
#19192=CARTESIAN_POINT('',(0.,-0.53,1.));
#19193=CARTESIAN_POINT('',(0.,-0.75,0.85));
#19194=CARTESIAN_POINT('',(0.,-0.53,1.));
#19195=CARTESIAN_POINT('',(22.,-0.75,0.85));
#19196=CARTESIAN_POINT('',(0.,-0.75,0.85));
#19197=CARTESIAN_POINT('',(22.,-0.53,1.));
#19198=CARTESIAN_POINT('',(22.,-0.53,1.));
#19199=CARTESIAN_POINT('',(0.,-0.53,1.));
#19200=CARTESIAN_POINT('Origin',(0.,-0.53,1.15));
#19201=CARTESIAN_POINT('',(0.,-0.53,1.15));
#19202=CARTESIAN_POINT('',(0.,-0.53,1.15));
#19203=CARTESIAN_POINT('',(22.,-0.53,1.15));
#19204=CARTESIAN_POINT('',(22.,-0.53,1.15));
#19205=CARTESIAN_POINT('',(0.,-0.53,1.15));
#19206=CARTESIAN_POINT('Origin',(0.,-0.75,1.3));
#19207=CARTESIAN_POINT('',(0.,-0.75,1.3));
#19208=CARTESIAN_POINT('',(0.,-0.75,1.3));
#19209=CARTESIAN_POINT('',(22.,-0.75,1.3));
#19210=CARTESIAN_POINT('',(22.,-0.75,1.3));
#19211=CARTESIAN_POINT('',(0.,-0.75,1.3));
#19212=CARTESIAN_POINT('Origin',(0.,-0.75,1.5));
#19213=CARTESIAN_POINT('',(0.,-0.75,1.5));
#19214=CARTESIAN_POINT('',(0.,-0.75,1.5));
#19215=CARTESIAN_POINT('',(22.,-0.75,1.5));
#19216=CARTESIAN_POINT('',(22.,-0.75,1.5));
#19217=CARTESIAN_POINT('',(0.,-0.75,1.5));
#19218=CARTESIAN_POINT('Origin',(0.,0.75,1.5));
#19219=CARTESIAN_POINT('',(0.,0.75,1.5));
#19220=CARTESIAN_POINT('',(0.,0.75,1.5));
#19221=CARTESIAN_POINT('',(22.,0.75,1.5));
#19222=CARTESIAN_POINT('',(22.,0.75,1.5));
#19223=CARTESIAN_POINT('',(0.,0.75,1.5));
#19224=CARTESIAN_POINT('Origin',(0.,0.75,1.3));
#19225=CARTESIAN_POINT('',(0.,0.75,1.3));
#19226=CARTESIAN_POINT('',(0.,0.75,1.3));
#19227=CARTESIAN_POINT('',(22.,0.75,1.3));
#19228=CARTESIAN_POINT('',(22.,0.75,1.3));
#19229=CARTESIAN_POINT('',(0.,0.75,1.3));
#19230=CARTESIAN_POINT('Origin',(0.,0.53,1.15));
#19231=CARTESIAN_POINT('',(0.,0.53,1.15));
#19232=CARTESIAN_POINT('',(0.,0.53,1.15));
#19233=CARTESIAN_POINT('',(22.,0.53,1.15));
#19234=CARTESIAN_POINT('',(22.,0.53,1.15));
#19235=CARTESIAN_POINT('',(0.,0.53,1.15));
#19236=CARTESIAN_POINT('Origin',(0.,0.53,1.));
#19237=CARTESIAN_POINT('',(0.,0.53,1.));
#19238=CARTESIAN_POINT('',(0.,0.53,1.));
#19239=CARTESIAN_POINT('',(22.,0.53,1.));
#19240=CARTESIAN_POINT('',(22.,0.53,1.));
#19241=CARTESIAN_POINT('',(0.,0.53,1.));
#19242=CARTESIAN_POINT('Origin',(0.,0.75,0.85));
#19243=CARTESIAN_POINT('',(0.,0.75,0.85));
#19244=CARTESIAN_POINT('',(0.,0.75,0.85));
#19245=CARTESIAN_POINT('',(22.,0.75,0.85));
#19246=CARTESIAN_POINT('',(22.,0.75,0.85));
#19247=CARTESIAN_POINT('',(0.,0.75,0.85));
#19248=CARTESIAN_POINT('Origin',(0.,0.75,0.));
#19249=CARTESIAN_POINT('',(0.,0.75,0.));
#19250=CARTESIAN_POINT('',(0.,0.75,0.));
#19251=CARTESIAN_POINT('',(22.,0.75,0.));
#19252=CARTESIAN_POINT('',(22.,0.75,0.));
#19253=CARTESIAN_POINT('',(0.,0.75,0.));
#19254=CARTESIAN_POINT('Origin',(0.,-0.75,0.));
#19255=CARTESIAN_POINT('',(0.,-0.75,0.));
#19256=CARTESIAN_POINT('',(0.,-0.75,0.));
#19257=CARTESIAN_POINT('',(22.,-0.75,0.));
#19258=CARTESIAN_POINT('',(22.,-0.75,0.));
#19259=CARTESIAN_POINT('',(0.,-0.75,0.));
#19260=CARTESIAN_POINT('Origin',(0.,-0.75,0.85));
#19261=CARTESIAN_POINT('',(0.,-0.75,0.85));
#19262=CARTESIAN_POINT('',(22.,-0.75,0.85));
#19263=CARTESIAN_POINT('Origin',(22.,0.,0.75));
#19264=CARTESIAN_POINT('Origin',(0.,0.,0.75));
#19265=CARTESIAN_POINT('',(0.,0.,0.));
#19266=CARTESIAN_POINT('',(0.,0.,0.));
#19267=CARTESIAN_POINT('Origin',(0.,0.,0.));
#19268=CARTESIAN_POINT('',(-1.070235,-0.308121667383195,-1.31065986708547E-16));
#19269=CARTESIAN_POINT('',(-1.31065986708547E-16,-0.308121667383195,1.070235));
#19270=CARTESIAN_POINT('Origin',(0.,-0.308121667383195,0.));
#19271=CARTESIAN_POINT('Origin',(0.,-0.308121667383195,0.));
#19272=CARTESIAN_POINT('',(-1.31065986708547E-16,0.308121667383195,1.070235));
#19273=CARTESIAN_POINT('Origin',(-1.34711147906209E-16,0.,1.1));
#19274=CARTESIAN_POINT('',(-1.070235,0.308121667383195,1.31065986708547E-16));
#19275=CARTESIAN_POINT('Origin',(0.,0.308121667383195,0.));
#19276=CARTESIAN_POINT('Origin',(0.,0.308121667383195,0.));
#19277=CARTESIAN_POINT('Origin',(0.,0.,0.));
#19278=CARTESIAN_POINT('',(-1.070235,0.5,-1.31065986708547E-16));
#19279=CARTESIAN_POINT('',(-1.070235,0.,-1.31065986708547E-16));
#19280=CARTESIAN_POINT('Origin',(0.,0.5,0.));
#19281=CARTESIAN_POINT('Origin',(0.,0.,0.));
#19282=CARTESIAN_POINT('',(-0.6,-0.44,-7.34788079488412E-17));
#19283=CARTESIAN_POINT('Origin',(0.,-0.44,0.));
#19284=CARTESIAN_POINT('',(-0.6,0.44,-7.34788079488412E-17));
#19285=CARTESIAN_POINT('',(-0.6,0.,-7.34788079488412E-17));
#19286=CARTESIAN_POINT('Origin',(0.,0.44,0.));
#19287=CARTESIAN_POINT('Origin',(0.,0.47,0.));
#19288=CARTESIAN_POINT('',(-0.66,0.5,-8.08266887437253E-17));
#19289=CARTESIAN_POINT('',(-0.63,0.47,-7.71527483462832E-17));
#19290=CARTESIAN_POINT('Origin',(0.,0.5,0.));
#19291=CARTESIAN_POINT('Origin',(1.070235,0.5,0.));
#19292=CARTESIAN_POINT('Origin',(0.,0.,0.));
#19293=CARTESIAN_POINT('',(-1.070235,-0.5,-1.31065986708547E-16));
#19294=CARTESIAN_POINT('Origin',(0.,-0.5,0.));
#19295=CARTESIAN_POINT('',(-1.070235,0.,-1.31065986708547E-16));
#19296=CARTESIAN_POINT('Origin',(0.66,-0.5,0.));
#19297=CARTESIAN_POINT('',(-0.66,-0.5,-8.08266887437253E-17));
#19298=CARTESIAN_POINT('Origin',(0.,-0.5,0.));
#19299=CARTESIAN_POINT('Origin',(0.,-0.47,0.));
#19300=CARTESIAN_POINT('',(-0.63,-0.47,-7.71527483462832E-17));
#19301=CARTESIAN_POINT('',(0.,0.,0.));
#19302=CARTESIAN_POINT('Origin',(0.,0.,0.));
#19303=CARTESIAN_POINT('',(-1.129765,0.308121667383195,-1.38356309103871E-16));
#19304=CARTESIAN_POINT('',(-1.38356309103871E-16,0.308121667383195,1.129765));
#19305=CARTESIAN_POINT('Origin',(0.,0.308121667383195,0.));
#19306=CARTESIAN_POINT('Origin',(0.,0.308121667383195,0.));
#19307=CARTESIAN_POINT('',(-1.38356309103871E-16,-0.308121667383195,1.129765));
#19308=CARTESIAN_POINT('Origin',(-1.34711147906209E-16,0.,1.1));
#19309=CARTESIAN_POINT('',(-1.129765,-0.308121667383195,1.38356309103871E-16));
#19310=CARTESIAN_POINT('Origin',(0.,-0.308121667383195,0.));
#19311=CARTESIAN_POINT('Origin',(0.,-0.308121667383195,0.));
#19312=CARTESIAN_POINT('Origin',(0.,0.,0.));
#19313=CARTESIAN_POINT('',(-1.129765,-0.5,-1.38356309103871E-16));
#19314=CARTESIAN_POINT('Origin',(0.,-0.5,0.));
#19315=CARTESIAN_POINT('',(-1.129765,0.,-1.38356309103871E-16));
#19316=CARTESIAN_POINT('Origin',(1.54,0.5,0.));
#19317=CARTESIAN_POINT('',(-1.54,0.5,-1.88595607068692E-16));
#19318=CARTESIAN_POINT('Origin',(0.,0.5,0.));
#19319=CARTESIAN_POINT('',(-1.129765,0.5,-1.38356309103871E-16));
#19320=CARTESIAN_POINT('Origin',(0.,0.5,0.));
#19321=CARTESIAN_POINT('Origin',(0.,0.47,0.));
#19322=CARTESIAN_POINT('',(-1.6,0.44,-1.95943487863577E-16));
#19323=CARTESIAN_POINT('Origin',(0.,0.44,0.));
#19324=CARTESIAN_POINT('',(-1.57,0.47,-1.92269547466134E-16));
#19325=CARTESIAN_POINT('Origin',(0.,0.,0.));
#19326=CARTESIAN_POINT('',(-1.6,-0.44,-1.95943487863577E-16));
#19327=CARTESIAN_POINT('Origin',(0.,-0.44,0.));
#19328=CARTESIAN_POINT('',(-1.6,0.,-1.95943487863577E-16));
#19329=CARTESIAN_POINT('Origin',(0.,-0.47,0.));
#19330=CARTESIAN_POINT('',(-1.54,-0.5,-1.88595607068692E-16));
#19331=CARTESIAN_POINT('Origin',(0.,-0.5,0.));
#19332=CARTESIAN_POINT('',(-1.57,-0.47,-1.92269547466134E-16));
#19333=CARTESIAN_POINT('Origin',(1.129765,-0.5,0.));
#19334=CARTESIAN_POINT('Origin',(0.,0.,0.));
#19335=CARTESIAN_POINT('',(-1.129765,0.,-1.38356309103871E-16));
#19336=CARTESIAN_POINT('',(0.,0.,0.));
#19337=CARTESIAN_POINT('Origin',(1.1,0.,0.));
#19338=CARTESIAN_POINT('',(1.1,-2.23201749654651E-33,0.29765));
#19339=CARTESIAN_POINT('',(1.1,-2.23201749654651E-33,-0.29765));
#19340=CARTESIAN_POINT('Origin',(1.1,0.,0.));
#19341=CARTESIAN_POINT('Origin',(0.685838782044607,0.,-0.860014630714833));
#19342=CARTESIAN_POINT('',(0.918550922801216,-5.31350540756609E-33,-0.674432891191581));
#19343=CARTESIAN_POINT('',(0.453126641287998,8.49470414473068E-34,-1.04559637023808));
#19344=CARTESIAN_POINT('Origin',(0.685838782044607,0.,-0.860014630714833));
#19345=CARTESIAN_POINT('Origin',(-0.244773027351946,0.,-1.07242070340001));
#19346=CARTESIAN_POINT('',(0.0454142657089739,-2.23201749654651E-33,-1.1386540593921));
#19347=CARTESIAN_POINT('',(-0.534960320412865,-2.23201749654651E-33,-1.00618734740791));
#19348=CARTESIAN_POINT('Origin',(-0.244773027351946,0.,-1.07242070340001));
#19349=CARTESIAN_POINT('Origin',(-0.991065754692661,0.,-0.477272113029314));
#19350=CARTESIAN_POINT('',(-0.86192025974432,8.49470414473067E-34,-0.745445496560469));
#19351=CARTESIAN_POINT('',(-1.120211249641,-5.31350540756609E-33,-0.209098729498159));
#19352=CARTESIAN_POINT('Origin',(-0.991065754692661,0.,-0.477272113029314));
#19353=CARTESIAN_POINT('Origin',(-0.991065754692661,0.,0.477272113029314));
#19354=CARTESIAN_POINT('',(-1.120211249641,-2.23201749654651E-33,0.209098729498159));
#19355=CARTESIAN_POINT('',(-0.86192025974432,-2.23201749654651E-33,0.745445496560469));
#19356=CARTESIAN_POINT('Origin',(-0.991065754692661,0.,0.477272113029314));
#19357=CARTESIAN_POINT('Origin',(-0.244773027351946,0.,1.07242070340001));
#19358=CARTESIAN_POINT('',(-0.534960320412866,-2.23201749654651E-33,1.00618734740791));
#19359=CARTESIAN_POINT('',(0.0454142657089737,-2.23201749654651E-33,1.1386540593921));
#19360=CARTESIAN_POINT('Origin',(-0.244773027351946,0.,1.07242070340001));
#19361=CARTESIAN_POINT('Origin',(0.685838782044607,0.,0.860014630714833));
#19362=CARTESIAN_POINT('',(0.453126641287998,-2.23201749654651E-33,1.04559637023808));
#19363=CARTESIAN_POINT('',(0.918550922801216,-2.23201749654651E-33,0.674432891191581));
#19364=CARTESIAN_POINT('Origin',(0.685838782044607,0.,0.860014630714833));
#19365=CARTESIAN_POINT('',(0.,0.,0.));
#19366=CARTESIAN_POINT('Origin',(0.685838782044607,0.,0.860014630714833));
#19367=CARTESIAN_POINT('',(0.413083465285518,-0.05953,0.993751811093549));
#19368=CARTESIAN_POINT('',(0.876916659919095,-0.05953,0.623857181492959));
#19369=CARTESIAN_POINT('Ctrl Pts',(0.413083465285518,-0.05953,0.993751811093549));
#19370=CARTESIAN_POINT('Ctrl Pts',(0.419070565453383,-0.0925528133349865,
0.991263089003441));
#19371=CARTESIAN_POINT('Ctrl Pts',(0.430199341854858,-0.124911173756694,
0.986608710139579));
#19372=CARTESIAN_POINT('Ctrl Pts',(0.457978755888596,-0.177924977804098,
0.973971221090534));
#19373=CARTESIAN_POINT('Ctrl Pts',(0.473077587363685,-0.199697230012983,
0.966820759530997));
#19374=CARTESIAN_POINT('Ctrl Pts',(0.507057380724533,-0.237895043532788,
0.949440676105255));
#19375=CARTESIAN_POINT('Ctrl Pts',(0.525933334162555,-0.254319232363049,
0.939198248544428));
#19376=CARTESIAN_POINT('Ctrl Pts',(0.564362943424238,-0.28018331644634,
0.916597376014514));
#19377=CARTESIAN_POINT('Ctrl Pts',(0.585840553788742,-0.29104845371857,
0.903141581680914));
#19378=CARTESIAN_POINT('Ctrl Pts',(0.629305439856167,-0.30527573347708,
0.873412008702649));
#19379=CARTESIAN_POINT('Ctrl Pts',(0.651278921914856,-0.308638795020976,
0.857118508332695));
#19380=CARTESIAN_POINT('Ctrl Pts',(0.690705563850638,-0.308638795020976,
0.825676810575914));
#19381=CARTESIAN_POINT('Ctrl Pts',(0.711480111898423,-0.30527573347708,
0.807879894508811));
#19382=CARTESIAN_POINT('Ctrl Pts',(0.750136149454208,-0.29104845371857,
0.772120216227122));
#19383=CARTESIAN_POINT('Ctrl Pts',(0.768033796848072,-0.28018331644634,
0.754175290318038));
#19384=CARTESIAN_POINT('Ctrl Pts',(0.798619410861634,-0.254319232363049,
0.721738358858166));
#19385=CARTESIAN_POINT('Ctrl Pts',(0.812805334167529,-0.237895043532788,
0.705614819529209));
#19386=CARTESIAN_POINT('Ctrl Pts',(0.837310877969633,-0.199697230012983,
0.676354402927683));
#19387=CARTESIAN_POINT('Ctrl Pts',(0.847641868610495,-0.177924977804098,
0.663225258065736));
#19388=CARTESIAN_POINT('Ctrl Pts',(0.866144010579847,-0.124911173756694,
0.638954437806245));
#19389=CARTESIAN_POINT('Ctrl Pts',(0.873158080166742,-0.0925528133349865,
0.62914037979579));
#19390=CARTESIAN_POINT('Ctrl Pts',(0.876916659919095,-0.05953,0.623857181492959));
#19391=CARTESIAN_POINT('',(0.437601487681057,-0.05953,1.03511272300331));
#19392=CARTESIAN_POINT('Origin',(0.685838782044607,-0.05953,0.860014630714833));
#19393=CARTESIAN_POINT('',(0.911784794170997,-0.05953,0.656964154625313));
#19394=CARTESIAN_POINT('Ctrl Pts',(0.911784794170998,-0.0595300000000001,
0.656964154625312));
#19395=CARTESIAN_POINT('Ctrl Pts',(0.909827729890942,-0.0762225747374255,
0.659680317203144));
#19396=CARTESIAN_POINT('Ctrl Pts',(0.907004864562642,-0.0928409665394228,
0.663576540841106));
#19397=CARTESIAN_POINT('Ctrl Pts',(0.895234408667242,-0.144299303100741,
0.679480524217551));
#19398=CARTESIAN_POINT('Ctrl Pts',(0.882797231409153,-0.177024326825049,
0.695831250979106));
#19399=CARTESIAN_POINT('Ctrl Pts',(0.854332839576145,-0.227269801620064,
0.73042219438957));
#19400=CARTESIAN_POINT('Ctrl Pts',(0.834863020612702,-0.251265615809407,
0.752807465209441));
#19401=CARTESIAN_POINT('Ctrl Pts',(0.800439809856111,-0.279889827963178,
0.789147407129766));
#19402=CARTESIAN_POINT('Ctrl Pts',(0.781998747691871,-0.290879136862659,
0.80756613568454));
#19403=CARTESIAN_POINT('Ctrl Pts',(0.742239891936898,-0.305251990234487,
0.844254137480382));
#19404=CARTESIAN_POINT('Ctrl Pts',(0.720906778729541,-0.308638795020976,
0.862505527716294));
#19405=CARTESIAN_POINT('Ctrl Pts',(0.680463863683392,-0.308638795020976,
0.894757676234429));
#19406=CARTESIAN_POINT('Ctrl Pts',(0.657923009631182,-0.305251990234488,
0.91149460735272));
#19407=CARTESIAN_POINT('Ctrl Pts',(0.613307674922609,-0.290879136862659,
0.942092777160053));
#19408=CARTESIAN_POINT('Ctrl Pts',(0.591247219971725,-0.279889827963178,
0.955972930713954));
#19409=CARTESIAN_POINT('Ctrl Pts',(0.548158511259202,-0.251265615809407,
0.981446681891443));
#19410=CARTESIAN_POINT('Ctrl Pts',(0.522002043615455,-0.227269801620063,
0.995447160474328));
#19411=CARTESIAN_POINT('Ctrl Pts',(0.481944444320713,-0.177024326825049,
1.01550068154148));
#19412=CARTESIAN_POINT('Ctrl Pts',(0.463236132117164,-0.14429930310074,
1.0239876538093));
#19413=CARTESIAN_POINT('Ctrl Pts',(0.445111721969657,-0.0928409665394226,
1.03192403056628));
#19414=CARTESIAN_POINT('Ctrl Pts',(0.440685038163619,-0.0762225747374254,
1.03380912944435));
#19415=CARTESIAN_POINT('Ctrl Pts',(0.437601487681056,-0.05953,1.03511272300331));
#19416=CARTESIAN_POINT('Origin',(0.685838782044607,-0.05953,0.860014630714833));
#19417=CARTESIAN_POINT('Origin',(0.,-0.208355,0.));
#19418=CARTESIAN_POINT('',(0.0548532617164168,-0.05953,1.12247250791415));
#19419=CARTESIAN_POINT('Origin',(0.,-0.05953,0.));
#19420=CARTESIAN_POINT('',(-0.536443649899848,-0.05953,0.987512846410683));
#19421=CARTESIAN_POINT('Ctrl Pts',(0.0548532617164173,-0.0595300000000001,
1.12247250791414));
#19422=CARTESIAN_POINT('Ctrl Pts',(0.05150947068137,-0.0762225747374254,
1.12263591311425));
#19423=CARTESIAN_POINT('Ctrl Pts',(0.0467032526342597,-0.0928409665394227,
1.12285816383385));
#19424=CARTESIAN_POINT('Ctrl Pts',(0.0269302585198975,-0.144299303100741,
1.12357162229597));
#19425=CARTESIAN_POINT('Ctrl Pts',(0.006392292392153,-0.177024326825049,
1.12404235695137));
#19426=CARTESIAN_POINT('Ctrl Pts',(-0.0383992541984087,-0.227269801620063,
1.12335509974011));
#19427=CARTESIAN_POINT('Ctrl Pts',(-0.0680399972366993,-0.251265615809407,
1.12208997038458));
#19428=CARTESIAN_POINT('Ctrl Pts',(-0.117914228755037,-0.279889827963178,
1.1178344036749));
#19429=CARTESIAN_POINT('Ctrl Pts',(-0.14381238480104,-0.290879136862659,
1.11490049012186));
#19430=CARTESIAN_POINT('Ctrl Pts',(-0.19728546073067,-0.305251990234488,
1.10669035995599));
#19431=CARTESIAN_POINT('Ctrl Pts',(-0.224855950742601,-0.308638795020976,
1.10139101611326));
#19432=CARTESIAN_POINT('Ctrl Pts',(-0.275287440920027,-0.308638795020976,
1.0898803575765));
#19433=CARTESIAN_POINT('Ctrl Pts',(-0.302426893214945,-0.305251990234488,
1.08269251410343));
#19434=CARTESIAN_POINT('Ctrl Pts',(-0.35416671187353,-0.290879136862659,
1.06688848765783));
#19435=CARTESIAN_POINT('Ctrl Pts',(-0.3787731215897,-0.279889827963178,
1.05829506364875));
#19436=CARTESIAN_POINT('Ctrl Pts',(-0.425554672694338,-0.251265615809407,
1.04048957871266));
#19437=CARTESIAN_POINT('Ctrl Pts',(-0.452808978448581,-0.227269801620063,
1.02876878445619));
#19438=CARTESIAN_POINT('Ctrl Pts',(-0.493462957200432,-0.177024326825049,
1.0099536580922));
#19439=CARTESIAN_POINT('Ctrl Pts',(-0.511762781179148,-0.14429930310074,
1.00061845128527));
#19440=CARTESIAN_POINT('Ctrl Pts',(-0.529268075276157,-0.0928409665394226,
0.991396466802468));
#19441=CARTESIAN_POINT('Ctrl Pts',(-0.533501897135713,-0.0762225747374254,
0.989110885965947));
#19442=CARTESIAN_POINT('Ctrl Pts',(-0.536443649899848,-0.0595300000000001,
0.987512846410683));
#19443=CARTESIAN_POINT('',(-0.843383895613249,-0.05953,0.742736168477219));
#19444=CARTESIAN_POINT('Origin',(0.,-0.05953,0.));
#19445=CARTESIAN_POINT('',(-1.10653577764992,-0.05953,0.196295654879792));
#19446=CARTESIAN_POINT('Ctrl Pts',(-0.843383895613249,-0.0595300000000001,
0.742736168477219));
#19447=CARTESIAN_POINT('Ctrl Pts',(-0.84559647055299,-0.0762225747374255,
0.740223768851062));
#19448=CARTESIAN_POINT('Ctrl Pts',(-0.848766861100456,-0.0928409665394227,
0.736604687327351));
#19449=CARTESIAN_POINT('Ctrl Pts',(-0.861652925570091,-0.144299303100741,
0.721590372101268));
#19450=CARTESIAN_POINT('Ctrl Pts',(-0.87482617317514,-0.177024326825049,
0.705826641853758));
#19451=CARTESIAN_POINT('Ctrl Pts',(-0.902215926359523,-0.227269801620063,
0.670378702718353));
#19452=CARTESIAN_POINT('Ctrl Pts',(-0.919707509403859,-0.251265615809407,
0.646415841396062));
#19453=CARTESIAN_POINT('Ctrl Pts',(-0.947476448101718,-0.279889827963178,
0.604769294586516));
#19454=CARTESIAN_POINT('Ctrl Pts',(-0.961329858300736,-0.290879136862659,
0.582692035672022));
#19455=CARTESIAN_POINT('Ctrl Pts',(-0.988250837578047,-0.305251990234488,
0.535766169015486));
#19456=CARTESIAN_POINT('Ctrl Pts',(-1.00129756308006,-0.308638795020976,
0.510906605094603));
#19457=CARTESIAN_POINT('Ctrl Pts',(-1.02374168767024,-0.308638795020976,
0.46430090015576));
#19458=CARTESIAN_POINT('Ctrl Pts',(-1.03504317708586,-0.305251990234488,
0.438600874831839));
#19459=CARTESIAN_POINT('Ctrl Pts',(-1.05494634094458,-0.290879136862659,
0.388295406390235));
#19460=CARTESIAN_POINT('Ctrl Pts',(-1.06356957703048,-0.279889827963178,
0.363699428370917));
#19461=CARTESIAN_POINT('Ctrl Pts',(-1.0788165083757,-0.251265615809407,
0.316022600643821));
#19462=CARTESIAN_POINT('Ctrl Pts',(-1.08664560412098,-0.227269801620063,
0.287406530683752));
#19463=CARTESIAN_POINT('Ctrl Pts',(-1.09728268713976,-0.177024326825049,
0.243890930799337));
#19464=CARTESIAN_POINT('Ctrl Pts',(-1.10139388218929,-0.144299303100741,
0.22376314604679));
#19465=CARTESIAN_POINT('Ctrl Pts',(-1.10509821673782,-0.0928409665394227,
0.204327142733961));
#19466=CARTESIAN_POINT('Ctrl Pts',(-1.10595102243643,-0.0762225747374254,
0.199591971170104));
#19467=CARTESIAN_POINT('Ctrl Pts',(-1.10653577764992,-0.0595300000000001,
0.196295654879792));
#19468=CARTESIAN_POINT('',(-1.123812,-0.05953,1.37627276864339E-16));
#19469=CARTESIAN_POINT('Origin',(0.,-0.05953,0.));
#19470=CARTESIAN_POINT('',(-1.123812,-0.35718,1.37627276864339E-16));
#19471=CARTESIAN_POINT('',(-1.123812,-0.208355,1.37627276864339E-16));
#19472=CARTESIAN_POINT('Origin',(0.,-0.35718,0.));
#19473=CARTESIAN_POINT('',(-1.10653577764992,-0.05953,-0.196295654879793));
#19474=CARTESIAN_POINT('Origin',(0.,-0.05953,0.));
#19475=CARTESIAN_POINT('',(-0.843383895613249,-0.05953,-0.742736168477219));
#19476=CARTESIAN_POINT('Ctrl Pts',(-1.10653577764992,-0.0595300000000001,
-0.196295654879792));
#19477=CARTESIAN_POINT('Ctrl Pts',(-1.10595102243643,-0.0762225747374255,
-0.199591971170104));
#19478=CARTESIAN_POINT('Ctrl Pts',(-1.10509821673782,-0.0928409665394228,
-0.204327142733962));
#19479=CARTESIAN_POINT('Ctrl Pts',(-1.10139388218929,-0.144299303100741,
-0.22376314604679));
#19480=CARTESIAN_POINT('Ctrl Pts',(-1.09728268713976,-0.177024326825049,
-0.243890930799338));
#19481=CARTESIAN_POINT('Ctrl Pts',(-1.08664560412098,-0.227269801620063,
-0.287406530683753));
#19482=CARTESIAN_POINT('Ctrl Pts',(-1.0788165083757,-0.251265615809407,
-0.316022600643821));
#19483=CARTESIAN_POINT('Ctrl Pts',(-1.06356957703048,-0.279889827963178,
-0.363699428370918));
#19484=CARTESIAN_POINT('Ctrl Pts',(-1.05494634094458,-0.290879136862659,
-0.388295406390235));
#19485=CARTESIAN_POINT('Ctrl Pts',(-1.03504317708586,-0.305251990234488,
-0.438600874831839));
#19486=CARTESIAN_POINT('Ctrl Pts',(-1.02374168767024,-0.308638795020976,
-0.46430090015576));
#19487=CARTESIAN_POINT('Ctrl Pts',(-1.00129756308006,-0.308638795020976,
-0.510906605094603));
#19488=CARTESIAN_POINT('Ctrl Pts',(-0.988250837578047,-0.305251990234488,
-0.535766169015486));
#19489=CARTESIAN_POINT('Ctrl Pts',(-0.961329858300736,-0.290879136862659,
-0.582692035672022));
#19490=CARTESIAN_POINT('Ctrl Pts',(-0.947476448101718,-0.279889827963178,
-0.604769294586516));
#19491=CARTESIAN_POINT('Ctrl Pts',(-0.919707509403859,-0.251265615809407,
-0.646415841396062));
#19492=CARTESIAN_POINT('Ctrl Pts',(-0.902215926359523,-0.227269801620064,
-0.670378702718353));
#19493=CARTESIAN_POINT('Ctrl Pts',(-0.87482617317514,-0.177024326825049,
-0.705826641853758));
#19494=CARTESIAN_POINT('Ctrl Pts',(-0.861652925570091,-0.144299303100741,
-0.721590372101268));
#19495=CARTESIAN_POINT('Ctrl Pts',(-0.848766861100456,-0.0928409665394229,
-0.736604687327351));
#19496=CARTESIAN_POINT('Ctrl Pts',(-0.84559647055299,-0.0762225747374255,
-0.740223768851063));
#19497=CARTESIAN_POINT('Ctrl Pts',(-0.843383895613249,-0.0595300000000001,
-0.742736168477219));
#19498=CARTESIAN_POINT('',(-0.536443649899847,-0.05953,-0.987512846410683));
#19499=CARTESIAN_POINT('Origin',(0.,-0.05953,0.));
#19500=CARTESIAN_POINT('',(0.0548532617164172,-0.05953,-1.12247250791415));
#19501=CARTESIAN_POINT('Ctrl Pts',(-0.536443649899848,-0.0595300000000001,
-0.987512846410683));
#19502=CARTESIAN_POINT('Ctrl Pts',(-0.533501897135712,-0.0762225747374254,
-0.989110885965947));
#19503=CARTESIAN_POINT('Ctrl Pts',(-0.529268075276156,-0.0928409665394227,
-0.991396466802469));
#19504=CARTESIAN_POINT('Ctrl Pts',(-0.511762781179147,-0.144299303100741,
-1.00061845128527));
#19505=CARTESIAN_POINT('Ctrl Pts',(-0.493462957200432,-0.177024326825049,
-1.0099536580922));
#19506=CARTESIAN_POINT('Ctrl Pts',(-0.45280897844858,-0.227269801620063,
-1.02876878445619));
#19507=CARTESIAN_POINT('Ctrl Pts',(-0.425554672694337,-0.251265615809407,
-1.04048957871266));
#19508=CARTESIAN_POINT('Ctrl Pts',(-0.3787731215897,-0.279889827963178,
-1.05829506364875));
#19509=CARTESIAN_POINT('Ctrl Pts',(-0.354166711873529,-0.290879136862659,
-1.06688848765783));
#19510=CARTESIAN_POINT('Ctrl Pts',(-0.302426893214944,-0.305251990234488,
-1.08269251410343));
#19511=CARTESIAN_POINT('Ctrl Pts',(-0.275287440920027,-0.308638795020976,
-1.0898803575765));
#19512=CARTESIAN_POINT('Ctrl Pts',(-0.224855950742601,-0.308638795020976,
-1.10139101611326));
#19513=CARTESIAN_POINT('Ctrl Pts',(-0.19728546073067,-0.305251990234488,
-1.10669035995599));
#19514=CARTESIAN_POINT('Ctrl Pts',(-0.143812384801039,-0.290879136862659,
-1.11490049012186));
#19515=CARTESIAN_POINT('Ctrl Pts',(-0.117914228755037,-0.279889827963178,
-1.1178344036749));
#19516=CARTESIAN_POINT('Ctrl Pts',(-0.0680399972366989,-0.251265615809407,
-1.12208997038458));
#19517=CARTESIAN_POINT('Ctrl Pts',(-0.0383992541984084,-0.227269801620063,
-1.12335509974011));
#19518=CARTESIAN_POINT('Ctrl Pts',(0.00639229239215326,-0.177024326825049,
-1.12404235695137));
#19519=CARTESIAN_POINT('Ctrl Pts',(0.0269302585198977,-0.144299303100741,
-1.12357162229597));
#19520=CARTESIAN_POINT('Ctrl Pts',(0.04670325263426,-0.0928409665394228,
-1.12285816383385));
#19521=CARTESIAN_POINT('Ctrl Pts',(0.0515094706813703,-0.0762225747374255,
-1.12263591311425));
#19522=CARTESIAN_POINT('Ctrl Pts',(0.0548532617164176,-0.0595300000000001,
-1.12247250791414));
#19523=CARTESIAN_POINT('',(0.437601487681057,-0.05953,-1.03511272300331));
#19524=CARTESIAN_POINT('Origin',(0.,-0.05953,0.));
#19525=CARTESIAN_POINT('',(0.911784794170997,-0.05953,-0.656964154625313));
#19526=CARTESIAN_POINT('Ctrl Pts',(0.437601487681056,-0.0595300000000001,
-1.03511272300331));
#19527=CARTESIAN_POINT('Ctrl Pts',(0.440685038163619,-0.0762225747374255,
-1.03380912944435));
#19528=CARTESIAN_POINT('Ctrl Pts',(0.445111721969657,-0.0928409665394228,
-1.03192403056628));
#19529=CARTESIAN_POINT('Ctrl Pts',(0.463236132117164,-0.144299303100741,
-1.0239876538093));
#19530=CARTESIAN_POINT('Ctrl Pts',(0.481944444320713,-0.177024326825049,
-1.01550068154148));
#19531=CARTESIAN_POINT('Ctrl Pts',(0.522002043615455,-0.227269801620064,
-0.995447160474328));
#19532=CARTESIAN_POINT('Ctrl Pts',(0.548158511259203,-0.251265615809407,
-0.981446681891443));
#19533=CARTESIAN_POINT('Ctrl Pts',(0.591247219971725,-0.279889827963178,
-0.955972930713954));
#19534=CARTESIAN_POINT('Ctrl Pts',(0.613307674922609,-0.290879136862659,
-0.942092777160053));
#19535=CARTESIAN_POINT('Ctrl Pts',(0.657923009631182,-0.305251990234487,
-0.91149460735272));
#19536=CARTESIAN_POINT('Ctrl Pts',(0.680463863683393,-0.308638795020976,
-0.894757676234429));
#19537=CARTESIAN_POINT('Ctrl Pts',(0.720906778729542,-0.308638795020976,
-0.862505527716294));
#19538=CARTESIAN_POINT('Ctrl Pts',(0.742239891936899,-0.305251990234488,
-0.844254137480381));
#19539=CARTESIAN_POINT('Ctrl Pts',(0.781998747691872,-0.290879136862659,
-0.80756613568454));
#19540=CARTESIAN_POINT('Ctrl Pts',(0.800439809856112,-0.279889827963178,
-0.789147407129765));
#19541=CARTESIAN_POINT('Ctrl Pts',(0.834863020612702,-0.251265615809407,
-0.752807465209441));
#19542=CARTESIAN_POINT('Ctrl Pts',(0.854332839576145,-0.227269801620064,
-0.73042219438957));
#19543=CARTESIAN_POINT('Ctrl Pts',(0.882797231409153,-0.177024326825049,
-0.695831250979106));
#19544=CARTESIAN_POINT('Ctrl Pts',(0.895234408667242,-0.144299303100741,
-0.679480524217551));
#19545=CARTESIAN_POINT('Ctrl Pts',(0.907004864562642,-0.0928409665394228,
-0.663576540841106));
#19546=CARTESIAN_POINT('Ctrl Pts',(0.909827729890942,-0.0762225747374256,
-0.659680317203144));
#19547=CARTESIAN_POINT('Ctrl Pts',(0.911784794170998,-0.0595300000000001,
-0.656964154625312));
#19548=CARTESIAN_POINT('',(1.08212377959455,-0.05953,-0.303251606722892));
#19549=CARTESIAN_POINT('Origin',(0.,-0.05953,0.));
#19550=CARTESIAN_POINT('',(1.08212377959455,-0.05953,0.303251606722892));
#19551=CARTESIAN_POINT('Ctrl Pts',(1.08212377959455,-0.0595300000000001,
-0.303251606722892));
#19552=CARTESIAN_POINT('Ctrl Pts',(1.0830271513892,-0.0762225747374255,
-0.300028012588062));
#19553=CARTESIAN_POINT('Ctrl Pts',(1.08431331394788,-0.0928409665394228,
-0.2953917518996));
#19554=CARTESIAN_POINT('Ctrl Pts',(1.08940878963422,-0.144299303100741,
-0.276273267473431));
#19555=CARTESIAN_POINT('Ctrl Pts',(1.09443784939331,-0.177024326825049,
-0.256354979351213));
#19556=CARTESIAN_POINT('Ctrl Pts',(1.10373487993589,-0.227269801620064,
-0.212533521233765));
#19557=CARTESIAN_POINT('Ctrl Pts',(1.10909715583869,-0.251265615809407,
-0.183354415742157));
#19558=CARTESIAN_POINT('Ctrl Pts',(1.1160463456491,-0.279889827963178,-0.133783682657561));
#19559=CARTESIAN_POINT('Ctrl Pts',(1.11894887330541,-0.290879136862659,
-0.107881990270302));
#19560=CARTESIAN_POINT('Ctrl Pts',(1.12284346704144,-0.305251990234488,
-0.0539226701638766));
#19561=CARTESIAN_POINT('Ctrl Pts',(1.123812,-0.308638795020976,-0.025864214957475));
#19562=CARTESIAN_POINT('Ctrl Pts',(1.123812,-0.308638795020976,0.025864214957475));
#19563=CARTESIAN_POINT('Ctrl Pts',(1.12284346704144,-0.305251990234488,
0.0539226701638766));
#19564=CARTESIAN_POINT('Ctrl Pts',(1.11894887330541,-0.290879136862659,
0.107881990270302));
#19565=CARTESIAN_POINT('Ctrl Pts',(1.1160463456491,-0.279889827963178,0.133783682657561));
#19566=CARTESIAN_POINT('Ctrl Pts',(1.10909715583869,-0.251265615809407,
0.183354415742157));
#19567=CARTESIAN_POINT('Ctrl Pts',(1.10373487993589,-0.227269801620064,
0.212533521233765));
#19568=CARTESIAN_POINT('Ctrl Pts',(1.09443784939331,-0.177024326825049,
0.256354979351213));
#19569=CARTESIAN_POINT('Ctrl Pts',(1.08940878963422,-0.144299303100741,
0.276273267473431));
#19570=CARTESIAN_POINT('Ctrl Pts',(1.08431331394788,-0.0928409665394228,
0.2953917518996));
#19571=CARTESIAN_POINT('Ctrl Pts',(1.0830271513892,-0.0762225747374255,
0.300028012588062));
#19572=CARTESIAN_POINT('Ctrl Pts',(1.08212377959455,-0.0595300000000001,
0.303251606722892));
#19573=CARTESIAN_POINT('Origin',(0.,-0.05953,0.));
#19574=CARTESIAN_POINT('Origin',(0.,-0.05953,0.));
#19575=CARTESIAN_POINT('',(0.0589974094846122,-0.05953,1.07456964270265));
#19576=CARTESIAN_POINT('Origin',(0.,-0.05953,0.));
#19577=CARTESIAN_POINT('Origin',(-0.244773027351946,-0.05953,1.07242070340001));
#19578=CARTESIAN_POINT('Origin',(-0.244773027351946,0.,1.07242070340001));
#19579=CARTESIAN_POINT('',(-0.519393123750572,-0.05953,0.942555777842682));
#19580=CARTESIAN_POINT('Ctrl Pts',(-0.519393123750572,-0.05953,0.942555777842682));
#19581=CARTESIAN_POINT('Ctrl Pts',(-0.513714466572041,-0.0925528133349865,
0.945684988399766));
#19582=CARTESIAN_POINT('Ctrl Pts',(-0.503136848051455,-0.124911173756694,
0.951483858396181));
#19583=CARTESIAN_POINT('Ctrl Pts',(-0.47593627990192,-0.177924977804098,
0.965323333309091));
#19584=CARTESIAN_POINT('Ctrl Pts',(-0.460931856495794,-0.199697230012983,
0.972669835243841));
#19585=CARTESIAN_POINT('Ctrl Pts',(-0.426157505475872,-0.237895043532788,
0.988400002689705));
#19586=CARTESIAN_POINT('Ctrl Pts',(-0.406380688682952,-0.254319232363049,
0.996771768218699));
#19587=CARTESIAN_POINT('Ctrl Pts',(-0.364750145543744,-0.28018331644634,
1.01272583306292));
#19588=CARTESIAN_POINT('Ctrl Pts',(-0.340838910881557,-0.29104845371857,
1.02112815447116));
#19589=CARTESIAN_POINT('Ctrl Pts',(-0.290495481564827,-0.30527573347708,
1.036574285215));
#19590=CARTESIAN_POINT('Ctrl Pts',(-0.264056468041074,-0.308638795020976,
1.04359501395068));
#19591=CARTESIAN_POINT('Ctrl Pts',(-0.214892249704082,-0.308638795020976,
1.05481642595959));
#19592=CARTESIAN_POINT('Ctrl Pts',(-0.188025341585962,-0.30527573347708,
1.05996242598502));
#19593=CARTESIAN_POINT('Ctrl Pts',(-0.135965654106109,-0.29104845371857,
1.06788913840721));
#19594=CARTESIAN_POINT('Ctrl Pts',(-0.110776745452494,-0.28018331644634,
1.07069360430242));
#19595=CARTESIAN_POINT('Ctrl Pts',(-0.0663467128214646,-0.254319232363049,
1.07438230428002));
#19596=CARTESIAN_POINT('Ctrl Pts',(-0.0448960436540983,-0.237895043532788,
1.07542044338697));
#19597=CARTESIAN_POINT('Ctrl Pts',(-0.00674037211528124,-0.199697230012983,
1.07633607767727));
#19598=CARTESIAN_POINT('Ctrl Pts',(0.00996567398334777,-0.177924977804098,
1.07622728347683));
#19599=CARTESIAN_POINT('Ctrl Pts',(0.0404772621979741,-0.124911173756694,
1.07556023164702));
#19600=CARTESIAN_POINT('Ctrl Pts',(0.0525234025782719,-0.0925528133349865,
1.07492508698591));
#19601=CARTESIAN_POINT('Ctrl Pts',(0.0589974094846124,-0.05953,1.07456964270265));
#19602=CARTESIAN_POINT('Origin',(-0.244773027351946,-0.05953,1.07242070340001));
#19603=CARTESIAN_POINT('Origin',(0.,-0.05953,0.));
#19604=CARTESIAN_POINT('',(-0.803348093619616,-0.05953,0.716109245731214));
#19605=CARTESIAN_POINT('Origin',(0.,-0.05953,0.));
#19606=CARTESIAN_POINT('Origin',(-0.991065754692661,-0.05953,0.477272113029314));
#19607=CARTESIAN_POINT('Origin',(-0.991065754692661,0.,0.477272113029314));
#19608=CARTESIAN_POINT('',(-1.06075609691358,-0.05953,0.181596019242328));
#19609=CARTESIAN_POINT('Ctrl Pts',(-1.06075609691358,-0.05953,0.181596019242328));
#19610=CARTESIAN_POINT('Ctrl Pts',(-1.05966202740332,-0.0925528133349865,
0.187986803072856));
#19611=CARTESIAN_POINT('Ctrl Pts',(-1.05760072925372,-0.124911173756694,
0.199872254546857));
#19612=CARTESIAN_POINT('Ctrl Pts',(-1.05146158959546,-0.177924977804098,
0.22976728653846));
#19613=CARTESIAN_POINT('Ctrl Pts',(-1.04785021111757,-0.199697230012983,
0.246078686169301));
#19614=CARTESIAN_POINT('Ctrl Pts',(-1.03846709802406,-0.237895043532788,
0.283073967563097));
#19615=CARTESIAN_POINT('Ctrl Pts',(-1.03268176429485,-0.254319232363049,
0.303755815985685));
#19616=CARTESIAN_POINT('Ctrl Pts',(-1.01919893537026,-0.28018331644634,
0.346251081972725));
#19617=CARTESIAN_POINT('Ctrl Pts',(-1.01085972381132,-0.29104845371857,
0.370184399726282));
#19618=CARTESIAN_POINT('Ctrl Pts',(-0.99154738033959,-0.30527573347708,
0.419174982698463));
#19619=CARTESIAN_POINT('Ctrl Pts',(-0.980551951791748,-0.308638795020976,
0.444223188605045));
#19620=CARTESIAN_POINT('Ctrl Pts',(-0.958671816228589,-0.308638795020976,
0.489657758261848));
#19621=CARTESIAN_POINT('Ctrl Pts',(-0.945943877838127,-0.30527573347708,
0.51387163140139));
#19622=CARTESIAN_POINT('Ctrl Pts',(-0.91968254693063,-0.29104845371857,
0.559515758398093));
#19623=CARTESIAN_POINT('Ctrl Pts',(-0.906170138993533,-0.28018331644634,
0.580957796077825));
#19624=CARTESIAN_POINT('Ctrl Pts',(-0.8813524085237,-0.254319232363049,
0.617994461173994));
#19625=CARTESIAN_POINT('Ctrl Pts',(-0.868789784891799,-0.237895043532788,
0.635412538795143));
#19626=CARTESIAN_POINT('Ctrl Pts',(-0.845715984518854,-0.199697230012983,
0.66581473268113));
#19627=CARTESIAN_POINT('Ctrl Pts',(-0.835214876415962,-0.177924977804098,
0.678808213394124));
#19628=CARTESIAN_POINT('Ctrl Pts',(-0.815669690204649,-0.124911173756694,
0.702247233627224));
#19629=CARTESIAN_POINT('Ctrl Pts',(-0.807662468433796,-0.0925528133349865,
0.711269279199861));
#19630=CARTESIAN_POINT('Ctrl Pts',(-0.803348093619616,-0.05953,0.716109245731214));
#19631=CARTESIAN_POINT('Origin',(-0.991065754692661,-0.05953,0.477272113029314));
#19632=CARTESIAN_POINT('Origin',(0.,-0.05953,0.));
#19633=CARTESIAN_POINT('',(-1.076188,-0.05953,1.31795018948079E-16));
#19634=CARTESIAN_POINT('Origin',(0.,-0.05953,0.));
#19635=CARTESIAN_POINT('',(-1.06075609691358,-0.05953,-0.181596019242328));
#19636=CARTESIAN_POINT('Origin',(0.,-0.05953,0.));
#19637=CARTESIAN_POINT('Origin',(-0.991065754692661,-0.05953,-0.477272113029314));
#19638=CARTESIAN_POINT('Origin',(-0.991065754692661,0.,-0.477272113029314));
#19639=CARTESIAN_POINT('',(-0.803348093619616,-0.05953,-0.716109245731215));
#19640=CARTESIAN_POINT('Ctrl Pts',(-0.803348093619616,-0.05953,-0.716109245731215));
#19641=CARTESIAN_POINT('Ctrl Pts',(-0.807662468433795,-0.0925528133349865,
-0.711269279199862));
#19642=CARTESIAN_POINT('Ctrl Pts',(-0.815669690204649,-0.124911173756694,
-0.702247233627224));
#19643=CARTESIAN_POINT('Ctrl Pts',(-0.835214876415962,-0.177924977804098,
-0.678808213394124));
#19644=CARTESIAN_POINT('Ctrl Pts',(-0.845715984518854,-0.199697230012983,
-0.66581473268113));
#19645=CARTESIAN_POINT('Ctrl Pts',(-0.868789784891799,-0.237895043532788,
-0.635412538795143));
#19646=CARTESIAN_POINT('Ctrl Pts',(-0.8813524085237,-0.254319232363049,
-0.617994461173994));
#19647=CARTESIAN_POINT('Ctrl Pts',(-0.906170138993533,-0.28018331644634,
-0.580957796077826));
#19648=CARTESIAN_POINT('Ctrl Pts',(-0.91968254693063,-0.29104845371857,
-0.559515758398093));
#19649=CARTESIAN_POINT('Ctrl Pts',(-0.945943877838127,-0.30527573347708,
-0.51387163140139));
#19650=CARTESIAN_POINT('Ctrl Pts',(-0.958671816228589,-0.308638795020976,
-0.489657758261848));
#19651=CARTESIAN_POINT('Ctrl Pts',(-0.980551951791748,-0.308638795020976,
-0.444223188605045));
#19652=CARTESIAN_POINT('Ctrl Pts',(-0.99154738033959,-0.30527573347708,
-0.419174982698463));
#19653=CARTESIAN_POINT('Ctrl Pts',(-1.01085972381132,-0.29104845371857,
-0.370184399726282));
#19654=CARTESIAN_POINT('Ctrl Pts',(-1.01919893537026,-0.28018331644634,
-0.346251081972725));
#19655=CARTESIAN_POINT('Ctrl Pts',(-1.03268176429485,-0.254319232363049,
-0.303755815985685));
#19656=CARTESIAN_POINT('Ctrl Pts',(-1.03846709802406,-0.237895043532788,
-0.283073967563097));
#19657=CARTESIAN_POINT('Ctrl Pts',(-1.04785021111757,-0.199697230012983,
-0.246078686169302));
#19658=CARTESIAN_POINT('Ctrl Pts',(-1.05146158959546,-0.177924977804098,
-0.229767286538461));
#19659=CARTESIAN_POINT('Ctrl Pts',(-1.05760072925372,-0.124911173756694,
-0.199872254546858));
#19660=CARTESIAN_POINT('Ctrl Pts',(-1.05966202740332,-0.0925528133349864,
-0.187986803072857));
#19661=CARTESIAN_POINT('Ctrl Pts',(-1.06075609691358,-0.05953,-0.181596019242328));
#19662=CARTESIAN_POINT('Origin',(-0.991065754692661,-0.05953,-0.477272113029314));
#19663=CARTESIAN_POINT('Origin',(0.,-0.05953,0.));
#19664=CARTESIAN_POINT('',(-0.519393123750572,-0.05953,-0.942555777842682));
#19665=CARTESIAN_POINT('Origin',(0.,-0.05953,0.));
#19666=CARTESIAN_POINT('Origin',(-0.244773027351946,-0.05953,-1.07242070340001));
#19667=CARTESIAN_POINT('Origin',(-0.244773027351946,0.,-1.07242070340001));
#19668=CARTESIAN_POINT('',(0.0589974094846125,-0.05953,-1.07456964270265));
#19669=CARTESIAN_POINT('Ctrl Pts',(0.0589974094846127,-0.05953,-1.07456964270265));
#19670=CARTESIAN_POINT('Ctrl Pts',(0.0525234025782722,-0.0925528133349865,
-1.07492508698591));
#19671=CARTESIAN_POINT('Ctrl Pts',(0.0404772621979744,-0.124911173756694,
-1.07556023164702));
#19672=CARTESIAN_POINT('Ctrl Pts',(0.0099656739833481,-0.177924977804098,
-1.07622728347683));
#19673=CARTESIAN_POINT('Ctrl Pts',(-0.00674037211528096,-0.199697230012983,
-1.07633607767727));
#19674=CARTESIAN_POINT('Ctrl Pts',(-0.044896043654098,-0.237895043532788,
-1.07542044338697));
#19675=CARTESIAN_POINT('Ctrl Pts',(-0.0663467128214644,-0.254319232363049,
-1.07438230428002));
#19676=CARTESIAN_POINT('Ctrl Pts',(-0.110776745452493,-0.28018331644634,
-1.07069360430242));
#19677=CARTESIAN_POINT('Ctrl Pts',(-0.135965654106109,-0.29104845371857,
-1.06788913840721));
#19678=CARTESIAN_POINT('Ctrl Pts',(-0.188025341585962,-0.30527573347708,
-1.05996242598502));
#19679=CARTESIAN_POINT('Ctrl Pts',(-0.214892249704082,-0.308638795020976,
-1.05481642595959));
#19680=CARTESIAN_POINT('Ctrl Pts',(-0.264056468041074,-0.308638795020976,
-1.04359501395068));
#19681=CARTESIAN_POINT('Ctrl Pts',(-0.290495481564827,-0.30527573347708,
-1.036574285215));
#19682=CARTESIAN_POINT('Ctrl Pts',(-0.340838910881557,-0.291048453718569,
-1.02112815447116));
#19683=CARTESIAN_POINT('Ctrl Pts',(-0.364750145543744,-0.28018331644634,
-1.01272583306292));
#19684=CARTESIAN_POINT('Ctrl Pts',(-0.406380688682952,-0.254319232363049,
-0.996771768218699));
#19685=CARTESIAN_POINT('Ctrl Pts',(-0.426157505475872,-0.237895043532788,
-0.988400002689705));
#19686=CARTESIAN_POINT('Ctrl Pts',(-0.460931856495794,-0.199697230012983,
-0.972669835243841));
#19687=CARTESIAN_POINT('Ctrl Pts',(-0.475936279901919,-0.177924977804098,
-0.965323333309091));
#19688=CARTESIAN_POINT('Ctrl Pts',(-0.503136848051454,-0.124911173756694,
-0.951483858396181));
#19689=CARTESIAN_POINT('Ctrl Pts',(-0.513714466572041,-0.0925528133349865,
-0.945684988399766));
#19690=CARTESIAN_POINT('Ctrl Pts',(-0.519393123750572,-0.05953,-0.942555777842682));
#19691=CARTESIAN_POINT('Origin',(-0.244773027351946,-0.05953,-1.07242070340001));
#19692=CARTESIAN_POINT('Origin',(0.,-0.05953,0.));
#19693=CARTESIAN_POINT('',(0.413083465285518,-0.05953,-0.993751811093549));
#19694=CARTESIAN_POINT('Origin',(0.,-0.05953,0.));
#19695=CARTESIAN_POINT('Origin',(0.685838782044607,-0.05953,-0.860014630714833));
#19696=CARTESIAN_POINT('Origin',(0.685838782044607,0.,-0.860014630714833));
#19697=CARTESIAN_POINT('',(0.876916659919095,-0.05953,-0.623857181492959));
#19698=CARTESIAN_POINT('Ctrl Pts',(0.876916659919095,-0.05953,-0.623857181492958));
#19699=CARTESIAN_POINT('Ctrl Pts',(0.873158080166742,-0.0925528133349865,
-0.62914037979579));
#19700=CARTESIAN_POINT('Ctrl Pts',(0.866144010579847,-0.124911173756694,
-0.638954437806245));
#19701=CARTESIAN_POINT('Ctrl Pts',(0.847641868610495,-0.177924977804098,
-0.663225258065736));
#19702=CARTESIAN_POINT('Ctrl Pts',(0.837310877969633,-0.199697230012983,
-0.676354402927683));
#19703=CARTESIAN_POINT('Ctrl Pts',(0.81280533416753,-0.237895043532788,
-0.705614819529209));
#19704=CARTESIAN_POINT('Ctrl Pts',(0.798619410861634,-0.254319232363049,
-0.721738358858166));
#19705=CARTESIAN_POINT('Ctrl Pts',(0.768033796848072,-0.28018331644634,
-0.754175290318038));
#19706=CARTESIAN_POINT('Ctrl Pts',(0.750136149454208,-0.29104845371857,
-0.772120216227122));
#19707=CARTESIAN_POINT('Ctrl Pts',(0.711480111898423,-0.30527573347708,
-0.807879894508811));
#19708=CARTESIAN_POINT('Ctrl Pts',(0.690705563850638,-0.308638795020976,
-0.825676810575913));
#19709=CARTESIAN_POINT('Ctrl Pts',(0.651278921914856,-0.308638795020976,
-0.857118508332695));
#19710=CARTESIAN_POINT('Ctrl Pts',(0.629305439856167,-0.30527573347708,
-0.873412008702649));
#19711=CARTESIAN_POINT('Ctrl Pts',(0.585840553788742,-0.29104845371857,
-0.903141581680914));
#19712=CARTESIAN_POINT('Ctrl Pts',(0.564362943424239,-0.28018331644634,
-0.916597376014514));
#19713=CARTESIAN_POINT('Ctrl Pts',(0.525933334162556,-0.254319232363049,
-0.939198248544427));
#19714=CARTESIAN_POINT('Ctrl Pts',(0.507057380724533,-0.237895043532788,
-0.949440676105255));
#19715=CARTESIAN_POINT('Ctrl Pts',(0.473077587363686,-0.199697230012983,
-0.966820759530997));
#19716=CARTESIAN_POINT('Ctrl Pts',(0.457978755888596,-0.177924977804098,
-0.973971221090534));
#19717=CARTESIAN_POINT('Ctrl Pts',(0.430199341854858,-0.124911173756694,
-0.986608710139579));
#19718=CARTESIAN_POINT('Ctrl Pts',(0.419070565453384,-0.0925528133349865,
-0.991263089003441));
#19719=CARTESIAN_POINT('Ctrl Pts',(0.413083465285518,-0.05953,-0.993751811093549));
#19720=CARTESIAN_POINT('Origin',(0.685838782044607,-0.05953,-0.860014630714833));
#19721=CARTESIAN_POINT('Origin',(0.,-0.208355,0.));
#19722=CARTESIAN_POINT('',(-1.076188,-0.35718,1.31795018948079E-16));
#19723=CARTESIAN_POINT('Origin',(0.,-0.35718,0.));
#19724=CARTESIAN_POINT('',(-1.076188,-0.208355,1.31795018948079E-16));
#19725=CARTESIAN_POINT('',(1.03449977959455,-0.05953,0.296632461748266));
#19726=CARTESIAN_POINT('Origin',(0.,-0.05953,0.));
#19727=CARTESIAN_POINT('',(1.03449977959455,-0.05953,-0.296632461748266));
#19728=CARTESIAN_POINT('Ctrl Pts',(1.03449977959455,-0.05953,0.296632461748267));
#19729=CARTESIAN_POINT('Ctrl Pts',(1.03628691421076,-0.0925528133349865,
0.290399865505497));
#19730=CARTESIAN_POINT('Ctrl Pts',(1.03958665287714,-0.124911173756694,
0.278797079997872));
#19731=CARTESIAN_POINT('Ctrl Pts',(1.0470264474309,-0.177924977804098,0.249198913998601));
#19732=CARTESIAN_POINT('Ctrl Pts',(1.05084995891418,-0.199697230012983,
0.232935932341942));
#19733=CARTESIAN_POINT('Ctrl Pts',(1.05844771715377,-0.237895043532788,
0.195533155353269));
#19734=CARTESIAN_POINT('Ctrl Pts',(1.06220882929878,-0.254319232363049,
0.17438929156337));
#19735=CARTESIAN_POINT('Ctrl Pts',(1.06849922508772,-0.28018331644634,0.130252399648131));
#19736=CARTESIAN_POINT('Ctrl Pts',(1.07137013248666,-0.29104845371857,0.105070977154072));
#19737=CARTESIAN_POINT('Ctrl Pts',(1.07522652957392,-0.30527573347708,0.0525526752791107));
#19738=CARTESIAN_POINT('Ctrl Pts',(1.076188,-0.308638795020976,0.025214283908933));
#19739=CARTESIAN_POINT('Ctrl Pts',(1.076188,-0.308638795020976,-0.025214283908933));
#19740=CARTESIAN_POINT('Ctrl Pts',(1.07522652957392,-0.30527573347708,-0.0525526752791107));
#19741=CARTESIAN_POINT('Ctrl Pts',(1.07137013248666,-0.29104845371857,-0.105070977154072));
#19742=CARTESIAN_POINT('Ctrl Pts',(1.06849922508772,-0.28018331644634,-0.130252399648131));
#19743=CARTESIAN_POINT('Ctrl Pts',(1.06220882929878,-0.254319232363049,
-0.17438929156337));
#19744=CARTESIAN_POINT('Ctrl Pts',(1.05844771715377,-0.237895043532788,
-0.195533155353269));
#19745=CARTESIAN_POINT('Ctrl Pts',(1.05084995891418,-0.199697230012983,
-0.232935932341942));
#19746=CARTESIAN_POINT('Ctrl Pts',(1.0470264474309,-0.177924977804098,-0.249198913998601));
#19747=CARTESIAN_POINT('Ctrl Pts',(1.03958665287714,-0.124911173756694,
-0.278797079997872));
#19748=CARTESIAN_POINT('Ctrl Pts',(1.03628691421076,-0.0925528133349865,
-0.290399865505497));
#19749=CARTESIAN_POINT('Ctrl Pts',(1.03449977959455,-0.05953,-0.296632461748267));
#19750=CARTESIAN_POINT('Origin',(0.,-0.05953,0.));
#19751=CARTESIAN_POINT('Origin',(0.,-0.05953,0.));
#19752=CARTESIAN_POINT('Origin',(1.1,-0.05953,0.));
#19753=CARTESIAN_POINT('Origin',(1.1,0.,0.));
#19754=CARTESIAN_POINT('Origin',(1.1,-0.05953,0.));
#19755=CARTESIAN_POINT('Origin',(0.,-0.35718,0.));
#19756=CARTESIAN_POINT('Origin',(0.,-0.05953,0.));
#19757=CARTESIAN_POINT('',(0.,0.,0.));
#19758=CARTESIAN_POINT('Origin',(1.119765,0.495,0.));
#19759=CARTESIAN_POINT('',(-1.119765,0.495,-1.37131662304724E-16));
#19760=CARTESIAN_POINT('Origin',(0.,0.495,0.));
#19761=CARTESIAN_POINT('',(-1.085235,0.495,-1.32902956907268E-16));
#19762=CARTESIAN_POINT('Origin',(0.,0.495,0.));
#19763=CARTESIAN_POINT('Origin',(0.,0.4575,0.));
#19764=CARTESIAN_POINT('',(-1.119765,0.42,-1.37131662304724E-16));
#19765=CARTESIAN_POINT('Origin',(0.,0.42,0.));
#19766=CARTESIAN_POINT('',(-1.119765,0.4575,-1.37131662304724E-16));
#19767=CARTESIAN_POINT('Origin',(1.085235,0.42,0.));
#19768=CARTESIAN_POINT('',(-1.085235,0.42,-1.32902956907268E-16));
#19769=CARTESIAN_POINT('Origin',(0.,0.42,0.));
#19770=CARTESIAN_POINT('Origin',(0.,0.4575,0.));
#19771=CARTESIAN_POINT('',(-1.085235,0.4575,-1.32902956907268E-16));
#19772=CARTESIAN_POINT('Origin',(1.119765,-0.42,0.));
#19773=CARTESIAN_POINT('',(-1.119765,-0.42,-1.37131662304724E-16));
#19774=CARTESIAN_POINT('Origin',(0.,-0.42,0.));
#19775=CARTESIAN_POINT('',(-1.085235,-0.42,-1.32902956907268E-16));
#19776=CARTESIAN_POINT('Origin',(0.,-0.42,0.));
#19777=CARTESIAN_POINT('Origin',(0.,-0.4575,0.));
#19778=CARTESIAN_POINT('',(-1.119765,-0.495,-1.37131662304724E-16));
#19779=CARTESIAN_POINT('Origin',(0.,-0.495,0.));
#19780=CARTESIAN_POINT('',(-1.119765,-0.4575,-1.37131662304724E-16));
#19781=CARTESIAN_POINT('Origin',(1.085235,-0.495,0.));
#19782=CARTESIAN_POINT('',(-1.085235,-0.495,-1.32902956907268E-16));
#19783=CARTESIAN_POINT('Origin',(0.,-0.495,0.));
#19784=CARTESIAN_POINT('Origin',(0.,-0.4575,0.));
#19785=CARTESIAN_POINT('',(-1.085235,-0.4575,-1.32902956907268E-16));
#19786=CARTESIAN_POINT('',(0.,0.,0.));
#19787=CARTESIAN_POINT('',(0.,0.,0.));
#19788=CARTESIAN_POINT('',(0.,0.,0.));
#19789=CARTESIAN_POINT('',(0.,0.,0.));
#19790=CARTESIAN_POINT('',(0.,0.,0.));
#19791=CARTESIAN_POINT('',(0.,0.,0.));
#19792=CARTESIAN_POINT('',(0.,0.,0.));
#19793=CARTESIAN_POINT('Origin',(0.,0.,0.));
#19794=CARTESIAN_POINT('',(-1.63531,-0.410863395882378,-2.00267715711366E-16));
#19795=CARTESIAN_POINT('',(-2.00267715711366E-16,-0.410863395882378,1.63531));
#19796=CARTESIAN_POINT('Origin',(0.,-0.410863395882378,0.));
#19797=CARTESIAN_POINT('Origin',(0.,-0.410863395882378,0.));
#19798=CARTESIAN_POINT('',(-2.00267715711366E-16,0.410863395882378,1.63531));
#19799=CARTESIAN_POINT('Origin',(-2.05128338857182E-16,0.,1.675));
#19800=CARTESIAN_POINT('',(-1.63531,0.410863395882378,2.00267715711366E-16));
#19801=CARTESIAN_POINT('Origin',(0.,0.410863395882378,0.));
#19802=CARTESIAN_POINT('Origin',(0.,0.410863395882378,0.));
#19803=CARTESIAN_POINT('Origin',(0.,0.,0.));
#19804=CARTESIAN_POINT('',(-1.63531,0.7,-2.00267715711366E-16));
#19805=CARTESIAN_POINT('',(-1.63531,0.,-2.00267715711366E-16));
#19806=CARTESIAN_POINT('Origin',(0.,0.7,0.));
#19807=CARTESIAN_POINT('Origin',(0.,0.,0.));
#19808=CARTESIAN_POINT('',(-1.,-0.6,-1.22464679914735E-16));
#19809=CARTESIAN_POINT('Origin',(0.,-0.6,0.));
#19810=CARTESIAN_POINT('',(-1.,0.6,-1.22464679914735E-16));
#19811=CARTESIAN_POINT('',(-1.,0.,-1.22464679914735E-16));
#19812=CARTESIAN_POINT('Origin',(0.,0.6,0.));
#19813=CARTESIAN_POINT('Origin',(0.,0.65,0.));
#19814=CARTESIAN_POINT('',(-1.1,0.7,-1.34711147906209E-16));
#19815=CARTESIAN_POINT('',(-1.05,0.65,-1.28587913910472E-16));
#19816=CARTESIAN_POINT('Origin',(0.,0.7,0.));
#19817=CARTESIAN_POINT('Origin',(1.63531,0.7,0.));
#19818=CARTESIAN_POINT('Origin',(0.,0.,0.));
#19819=CARTESIAN_POINT('',(-1.63531,-0.7,-2.00267715711366E-16));
#19820=CARTESIAN_POINT('Origin',(0.,-0.7,0.));
#19821=CARTESIAN_POINT('',(-1.63531,0.,-2.00267715711366E-16));
#19822=CARTESIAN_POINT('Origin',(1.1,-0.7,0.));
#19823=CARTESIAN_POINT('',(-1.1,-0.7,-1.34711147906209E-16));
#19824=CARTESIAN_POINT('Origin',(0.,-0.7,0.));
#19825=CARTESIAN_POINT('Origin',(0.,-0.65,0.));
#19826=CARTESIAN_POINT('',(-1.05,-0.65,-1.28587913910472E-16));
#19827=CARTESIAN_POINT('',(0.,0.,0.));
#19828=CARTESIAN_POINT('Origin',(0.,0.,0.));
#19829=CARTESIAN_POINT('',(-1.71469,0.410863395882378,-2.09988962002998E-16));
#19830=CARTESIAN_POINT('',(-2.09988962002998E-16,0.410863395882378,1.71469));
#19831=CARTESIAN_POINT('Origin',(0.,0.410863395882378,0.));
#19832=CARTESIAN_POINT('Origin',(0.,0.410863395882378,0.));
#19833=CARTESIAN_POINT('',(-2.09988962002998E-16,-0.410863395882378,1.71469));
#19834=CARTESIAN_POINT('Origin',(-2.05128338857182E-16,0.,1.675));
#19835=CARTESIAN_POINT('',(-1.71469,-0.410863395882378,2.09988962002998E-16));
#19836=CARTESIAN_POINT('Origin',(0.,-0.410863395882378,0.));
#19837=CARTESIAN_POINT('Origin',(0.,-0.410863395882378,0.));
#19838=CARTESIAN_POINT('Origin',(0.,0.,0.));
#19839=CARTESIAN_POINT('',(-1.71469,-0.7,-2.09988962002998E-16));
#19840=CARTESIAN_POINT('Origin',(0.,-0.7,0.));
#19841=CARTESIAN_POINT('',(-1.71469,0.,-2.09988962002998E-16));
#19842=CARTESIAN_POINT('Origin',(2.25,0.7,0.));
#19843=CARTESIAN_POINT('',(-2.25,0.7,-2.75545529808154E-16));
#19844=CARTESIAN_POINT('Origin',(0.,0.7,0.));
#19845=CARTESIAN_POINT('',(-1.71469,0.7,-2.09988962002998E-16));
#19846=CARTESIAN_POINT('Origin',(0.,0.7,0.));
#19847=CARTESIAN_POINT('Origin',(0.,0.65,0.));
#19848=CARTESIAN_POINT('',(-2.35,0.6,-2.87791997799628E-16));
#19849=CARTESIAN_POINT('Origin',(0.,0.6,0.));
#19850=CARTESIAN_POINT('',(-2.3,0.65,-2.81668763803891E-16));
#19851=CARTESIAN_POINT('Origin',(0.,0.,0.));
#19852=CARTESIAN_POINT('',(-2.35,-0.6,-2.87791997799628E-16));
#19853=CARTESIAN_POINT('Origin',(0.,-0.6,0.));
#19854=CARTESIAN_POINT('',(-2.35,0.,-2.87791997799628E-16));
#19855=CARTESIAN_POINT('Origin',(0.,-0.65,0.));
#19856=CARTESIAN_POINT('',(-2.25,-0.7,-2.75545529808154E-16));
#19857=CARTESIAN_POINT('Origin',(0.,-0.7,0.));
#19858=CARTESIAN_POINT('',(-2.3,-0.65,-2.81668763803891E-16));
#19859=CARTESIAN_POINT('Origin',(1.71469,-0.7,0.));
#19860=CARTESIAN_POINT('Origin',(0.,0.,0.));
#19861=CARTESIAN_POINT('',(-1.71469,0.,-2.09988962002998E-16));
#19862=CARTESIAN_POINT('',(0.,0.,0.));
#19863=CARTESIAN_POINT('Origin',(1.675,0.,0.));
#19864=CARTESIAN_POINT('',(1.675,-2.97627328869245E-33,0.3969));
#19865=CARTESIAN_POINT('',(1.675,-2.97627328869245E-33,-0.3969));
#19866=CARTESIAN_POINT('Origin',(1.675,0.,0.));
#19867=CARTESIAN_POINT('Origin',(1.18440385848747,0.,-1.18440385848747));
#19868=CARTESIAN_POINT('',(1.46505453994041,3.1867025333467E-33,-0.903753177034526));
#19869=CARTESIAN_POINT('',(0.903753177034527,-9.13924911073161E-33,-1.46505453994041));
#19870=CARTESIAN_POINT('Origin',(1.18440385848747,0.,-1.18440385848747));
#19871=CARTESIAN_POINT('Origin',(1.02564169428591E-16,0.,-1.675));
#19872=CARTESIAN_POINT('',(0.3969,-2.97627328869246E-33,-1.675));
#19873=CARTESIAN_POINT('',(-0.3969,-2.97627328869245E-33,-1.675));
#19874=CARTESIAN_POINT('Origin',(1.02564169428591E-16,0.,-1.675));
#19875=CARTESIAN_POINT('Origin',(-1.18440385848747,0.,-1.18440385848747));
#19876=CARTESIAN_POINT('',(-0.903753177034526,3.1867025333467E-33,-1.46505453994041));
#19877=CARTESIAN_POINT('',(-1.46505453994041,-9.13924911073161E-33,-0.903753177034527));
#19878=CARTESIAN_POINT('Origin',(-1.18440385848747,0.,-1.18440385848747));
#19879=CARTESIAN_POINT('Origin',(-1.675,0.,-2.05128338857182E-16));
#19880=CARTESIAN_POINT('',(-1.675,-2.97627328869246E-33,-0.3969));
#19881=CARTESIAN_POINT('',(-1.675,-2.97627328869245E-33,0.3969));
#19882=CARTESIAN_POINT('Origin',(-1.675,0.,-2.05128338857182E-16));
#19883=CARTESIAN_POINT('Origin',(-1.18440385848747,0.,1.18440385848747));
#19884=CARTESIAN_POINT('',(-1.46505453994041,6.26819044436628E-33,0.903753177034526));
#19885=CARTESIAN_POINT('',(-0.903753177034527,-1.22207370217512E-32,1.46505453994041));
#19886=CARTESIAN_POINT('Origin',(-1.18440385848747,0.,1.18440385848747));
#19887=CARTESIAN_POINT('Origin',(-3.07692508285772E-16,0.,1.675));
#19888=CARTESIAN_POINT('',(-0.3969,-2.97627328869246E-33,1.675));
#19889=CARTESIAN_POINT('',(0.396899999999999,-2.97627328869245E-33,1.675));
#19890=CARTESIAN_POINT('Origin',(-3.07692508285772E-16,0.,1.675));
#19891=CARTESIAN_POINT('Origin',(1.18440385848747,0.,1.18440385848747));
#19892=CARTESIAN_POINT('',(0.903753177034526,9.34967835538585E-33,1.46505453994041));
#19893=CARTESIAN_POINT('',(1.46505453994041,-1.53022249327708E-32,0.903753177034527));
#19894=CARTESIAN_POINT('Origin',(1.18440385848747,0.,1.18440385848747));
#19895=CARTESIAN_POINT('',(0.,0.,0.));
#19896=CARTESIAN_POINT('Origin',(1.18440385848747,0.,1.18440385848747));
#19897=CARTESIAN_POINT('',(0.846804978391753,-0.07938,1.40825612658882));
#19898=CARTESIAN_POINT('',(1.40825612658882,-0.07938,0.846804978391754));
#19899=CARTESIAN_POINT('Ctrl Pts',(0.846804978391752,-0.0793800000000001,
1.40825612658882));
#19900=CARTESIAN_POINT('Ctrl Pts',(0.854205272175554,-0.123401821157026,
1.40380622184538));
#19901=CARTESIAN_POINT('Ctrl Pts',(0.867957148219441,-0.166543350814306,
1.39550172959303));
#19902=CARTESIAN_POINT('Ctrl Pts',(0.902193646979982,-0.237231147975234,
1.3735491215176));
#19903=CARTESIAN_POINT('Ctrl Pts',(0.920778333482564,-0.266264900654909,
1.36127834356734));
#19904=CARTESIAN_POINT('Ctrl Pts',(0.962485392528369,-0.317195968905306,
1.33211611256184));
#19905=CARTESIAN_POINT('Ctrl Pts',(0.985600426557816,-0.33909093068465,
1.31521005565926));
#19906=CARTESIAN_POINT('Ctrl Pts',(1.03253285680459,-0.373586846396559,
1.27866649102984));
#19907=CARTESIAN_POINT('Ctrl Pts',(1.05871835910697,-0.388086240756494,
1.25722555095714));
#19908=CARTESIAN_POINT('Ctrl Pts',(1.11153475808518,-0.407068917407805,
1.2107812086231));
#19909=CARTESIAN_POINT('Ctrl Pts',(1.13814686046673,-0.411552957311693,
1.18575674747573));
#19910=CARTESIAN_POINT('Ctrl Pts',(1.18575674747573,-0.411552957311693,
1.13814686046673));
#19911=CARTESIAN_POINT('Ctrl Pts',(1.2107812086231,-0.407068917407805,1.11153475808518));
#19912=CARTESIAN_POINT('Ctrl Pts',(1.25722555095713,-0.388086240756494,
1.05871835910697));
#19913=CARTESIAN_POINT('Ctrl Pts',(1.27866649102984,-0.373586846396559,
1.03253285680459));
#19914=CARTESIAN_POINT('Ctrl Pts',(1.31521005565926,-0.33909093068465,0.985600426557816));
#19915=CARTESIAN_POINT('Ctrl Pts',(1.33211611256184,-0.317195968905306,
0.962485392528369));
#19916=CARTESIAN_POINT('Ctrl Pts',(1.36127834356734,-0.266264900654909,
0.920778333482565));
#19917=CARTESIAN_POINT('Ctrl Pts',(1.3735491215176,-0.237231147975234,0.902193646979983));
#19918=CARTESIAN_POINT('Ctrl Pts',(1.39550172959303,-0.166543350814306,
0.867957148219442));
#19919=CARTESIAN_POINT('Ctrl Pts',(1.40380622184538,-0.123401821157026,
0.854205272175555));
#19920=CARTESIAN_POINT('Ctrl Pts',(1.40825612658882,-0.0793800000000001,
0.846804978391753));
#19921=CARTESIAN_POINT('',(0.886256117232623,-0.07938,1.45861320581289));
#19922=CARTESIAN_POINT('Origin',(1.18440385848747,-0.07938,1.18440385848747));
#19923=CARTESIAN_POINT('',(1.45861320581289,-0.07938,0.886256117232624));
#19924=CARTESIAN_POINT('Ctrl Pts',(1.45861320581289,-0.0793800000000001,
0.886256117232623));
#19925=CARTESIAN_POINT('Ctrl Pts',(1.45630208793976,-0.101649918886749,
0.890059788636852));
#19926=CARTESIAN_POINT('Ctrl Pts',(1.45296717977858,-0.123823518623746,
0.895520212222107));
#19927=CARTESIAN_POINT('Ctrl Pts',(1.43904931717599,-0.192480977588836,
0.917859913453975));
#19928=CARTESIAN_POINT('Ctrl Pts',(1.4243271592157,-0.236152929235938,0.940896403863072));
#19929=CARTESIAN_POINT('Ctrl Pts',(1.39055359345152,-0.303141259068212,
0.990027513266106));
#19930=CARTESIAN_POINT('Ctrl Pts',(1.36743459453896,-0.335108247315849,
1.02199477007745));
#19931=CARTESIAN_POINT('Ctrl Pts',(1.32643091652006,-0.373243761060364,
1.07446535104584));
#19932=CARTESIAN_POINT('Ctrl Pts',(1.30441816675528,-0.387888272594439,
1.10126842659597));
#19933=CARTESIAN_POINT('Ctrl Pts',(1.25681160160691,-0.407041111792943,
1.15530234155453));
#19934=CARTESIAN_POINT('Ctrl Pts',(1.23119764287622,-0.411552957311693,
1.18251418313119));
#19935=CARTESIAN_POINT('Ctrl Pts',(1.18251418313119,-0.411552957311693,
1.23119764287622));
#19936=CARTESIAN_POINT('Ctrl Pts',(1.15530234155453,-0.407041111792943,
1.25681160160691));
#19937=CARTESIAN_POINT('Ctrl Pts',(1.10126842659597,-0.387888272594439,
1.30441816675528));
#19938=CARTESIAN_POINT('Ctrl Pts',(1.07446535104584,-0.373243761060364,
1.32643091652006));
#19939=CARTESIAN_POINT('Ctrl Pts',(1.02199477007745,-0.335108247315848,
1.36743459453896));
#19940=CARTESIAN_POINT('Ctrl Pts',(0.990027513266105,-0.303141259068211,
1.39055359345152));
#19941=CARTESIAN_POINT('Ctrl Pts',(0.940896403863071,-0.236152929235937,
1.42432715921571));
#19942=CARTESIAN_POINT('Ctrl Pts',(0.917859913453974,-0.192480977588835,
1.43904931717599));
#19943=CARTESIAN_POINT('Ctrl Pts',(0.895520212222106,-0.123823518623745,
1.45296717977858));
#19944=CARTESIAN_POINT('Ctrl Pts',(0.890059788636851,-0.101649918886749,
1.45630208793976));
#19945=CARTESIAN_POINT('Ctrl Pts',(0.886256117232622,-0.0793800000000001,
1.45861320581289));
#19946=CARTESIAN_POINT('Origin',(1.18440385848747,-0.07938,1.18440385848747));
#19947=CARTESIAN_POINT('Origin',(0.,-0.27783,0.));
#19948=CARTESIAN_POINT('',(0.404717578595295,-0.07938,1.65807299932179));
#19949=CARTESIAN_POINT('Origin',(0.,-0.07938,0.));
#19950=CARTESIAN_POINT('',(-0.404717578595296,-0.07938,1.65807299932179));
#19951=CARTESIAN_POINT('Ctrl Pts',(0.404717578595296,-0.0793800000000001,
1.65807299932179));
#19952=CARTESIAN_POINT('Ctrl Pts',(0.400393769631747,-0.101649918886749,
1.65912839404491));
#19953=CARTESIAN_POINT('Ctrl Pts',(0.394174530911058,-0.123823518623745,
1.66063136041479));
#19954=CARTESIAN_POINT('Ctrl Pts',(0.368536561654407,-0.192480977588835,
1.66658649961961));
#19955=CARTESIAN_POINT('Ctrl Pts',(0.341837165343982,-0.236152929235937,
1.67246562047521));
#19956=CARTESIAN_POINT('Ctrl Pts',(0.283214707341173,-0.303141259068211,
1.68332504372461));
#19957=CARTESIAN_POINT('Ctrl Pts',(0.244262842368623,-0.335108247315849,
1.68958170688653));
#19958=CARTESIAN_POINT('Ctrl Pts',(0.178166559972324,-0.373243761060364,
1.69769003172132));
#19959=CARTESIAN_POINT('Ctrl Pts',(0.143648558862931,-0.387888272594439,
1.70107730356824));
#19960=CARTESIAN_POINT('Ctrl Pts',(0.0717778861362652,-0.407041111792943,
1.70562212620408));
#19961=CARTESIAN_POINT('Ctrl Pts',(0.0344244045173309,-0.411552957311693,
1.706752));
#19962=CARTESIAN_POINT('Ctrl Pts',(-0.0344244045173315,-0.411552957311693,
1.706752));
#19963=CARTESIAN_POINT('Ctrl Pts',(-0.0717778861362658,-0.407041111792943,
1.70562212620408));
#19964=CARTESIAN_POINT('Ctrl Pts',(-0.143648558862932,-0.387888272594439,
1.70107730356824));
#19965=CARTESIAN_POINT('Ctrl Pts',(-0.178166559972325,-0.373243761060364,
1.69769003172132));
#19966=CARTESIAN_POINT('Ctrl Pts',(-0.244262842368624,-0.335108247315849,
1.68958170688653));
#19967=CARTESIAN_POINT('Ctrl Pts',(-0.283214707341173,-0.303141259068212,
1.68332504372461));
#19968=CARTESIAN_POINT('Ctrl Pts',(-0.341837165343982,-0.236152929235937,
1.67246562047521));
#19969=CARTESIAN_POINT('Ctrl Pts',(-0.368536561654408,-0.192480977588835,
1.66658649961961));
#19970=CARTESIAN_POINT('Ctrl Pts',(-0.394174530911059,-0.123823518623745,
1.66063136041479));
#19971=CARTESIAN_POINT('Ctrl Pts',(-0.400393769631748,-0.101649918886749,
1.65912839404491));
#19972=CARTESIAN_POINT('Ctrl Pts',(-0.404717578595297,-0.0793800000000001,
1.65807299932179));
#19973=CARTESIAN_POINT('',(-0.886256117232624,-0.07938,1.45861320581289));
#19974=CARTESIAN_POINT('Origin',(0.,-0.07938,0.));
#19975=CARTESIAN_POINT('',(-1.45861320581289,-0.07938,0.886256117232623));
#19976=CARTESIAN_POINT('Ctrl Pts',(-0.886256117232623,-0.0793800000000001,
1.45861320581289));
#19977=CARTESIAN_POINT('Ctrl Pts',(-0.890059788636852,-0.101649918886749,
1.45630208793976));
#19978=CARTESIAN_POINT('Ctrl Pts',(-0.895520212222106,-0.123823518623745,
1.45296717977858));
#19979=CARTESIAN_POINT('Ctrl Pts',(-0.917859913453974,-0.192480977588835,
1.43904931717599));
#19980=CARTESIAN_POINT('Ctrl Pts',(-0.940896403863071,-0.236152929235937,
1.4243271592157));
#19981=CARTESIAN_POINT('Ctrl Pts',(-0.990027513266105,-0.303141259068211,
1.39055359345152));
#19982=CARTESIAN_POINT('Ctrl Pts',(-1.02199477007745,-0.335108247315848,
1.36743459453896));
#19983=CARTESIAN_POINT('Ctrl Pts',(-1.07446535104584,-0.373243761060364,
1.32643091652006));
#19984=CARTESIAN_POINT('Ctrl Pts',(-1.10126842659597,-0.387888272594439,
1.30441816675528));
#19985=CARTESIAN_POINT('Ctrl Pts',(-1.15530234155453,-0.407041111792943,
1.25681160160691));
#19986=CARTESIAN_POINT('Ctrl Pts',(-1.18251418313119,-0.411552957311693,
1.23119764287622));
#19987=CARTESIAN_POINT('Ctrl Pts',(-1.23119764287622,-0.411552957311693,
1.18251418313119));
#19988=CARTESIAN_POINT('Ctrl Pts',(-1.25681160160691,-0.407041111792943,
1.15530234155453));
#19989=CARTESIAN_POINT('Ctrl Pts',(-1.30441816675528,-0.387888272594439,
1.10126842659597));
#19990=CARTESIAN_POINT('Ctrl Pts',(-1.32643091652006,-0.373243761060365,
1.07446535104584));
#19991=CARTESIAN_POINT('Ctrl Pts',(-1.36743459453896,-0.335108247315849,
1.02199477007745));
#19992=CARTESIAN_POINT('Ctrl Pts',(-1.39055359345152,-0.303141259068212,
0.990027513266106));
#19993=CARTESIAN_POINT('Ctrl Pts',(-1.4243271592157,-0.236152929235938,
0.940896403863071));
#19994=CARTESIAN_POINT('Ctrl Pts',(-1.43904931717599,-0.192480977588836,
0.917859913453974));
#19995=CARTESIAN_POINT('Ctrl Pts',(-1.45296717977858,-0.123823518623746,
0.895520212222106));
#19996=CARTESIAN_POINT('Ctrl Pts',(-1.45630208793976,-0.101649918886749,
0.890059788636852));
#19997=CARTESIAN_POINT('Ctrl Pts',(-1.45861320581289,-0.0793800000000001,
0.886256117232623));
#19998=CARTESIAN_POINT('',(-1.65807299932179,-0.07938,0.404717578595295));
#19999=CARTESIAN_POINT('Origin',(0.,-0.07938,0.));
#20000=CARTESIAN_POINT('',(-1.706752,-0.411552957311693,2.08591827245526E-16));
#20001=CARTESIAN_POINT('Ctrl Pts',(-1.65807299932179,-0.0793800000000001,
0.404717578595296));
#20002=CARTESIAN_POINT('Ctrl Pts',(-1.65912839404491,-0.101649918886749,
0.400393769631747));
#20003=CARTESIAN_POINT('Ctrl Pts',(-1.66063136041479,-0.123823518623745,
0.394174530911058));
#20004=CARTESIAN_POINT('Ctrl Pts',(-1.66658649961961,-0.192480977588835,
0.368536561654407));
#20005=CARTESIAN_POINT('Ctrl Pts',(-1.67246562047521,-0.236152929235937,
0.341837165343982));
#20006=CARTESIAN_POINT('Ctrl Pts',(-1.68332504372461,-0.303141259068211,
0.283214707341173));
#20007=CARTESIAN_POINT('Ctrl Pts',(-1.68958170688653,-0.335108247315848,
0.244262842368623));
#20008=CARTESIAN_POINT('Ctrl Pts',(-1.69769003172132,-0.373243761060364,
0.178166559972324));
#20009=CARTESIAN_POINT('Ctrl Pts',(-1.70107730356824,-0.387888272594439,
0.143648558862931));
#20010=CARTESIAN_POINT('Ctrl Pts',(-1.70562212620408,-0.407041111792943,
0.0717778861362656));
#20011=CARTESIAN_POINT('Ctrl Pts',(-1.706752,-0.411552957311693,0.0344244045173313));
#20012=CARTESIAN_POINT('Ctrl Pts',(-1.706752,-0.411552957311693,2.08166817117217E-16));
#20013=CARTESIAN_POINT('',(-1.706752,-0.47628,2.09016837373834E-16));
#20014=CARTESIAN_POINT('',(-1.706752,-0.27783,2.09016837373834E-16));
#20015=CARTESIAN_POINT('Origin',(0.,-0.47628,0.));
#20016=CARTESIAN_POINT('',(-1.65807299932179,-0.07938,-0.404717578595296));
#20017=CARTESIAN_POINT('Ctrl Pts',(-1.706752,-0.411552957311693,2.0122792321331E-16));
#20018=CARTESIAN_POINT('Ctrl Pts',(-1.706752,-0.411552957311693,-0.0344244045173309));
#20019=CARTESIAN_POINT('Ctrl Pts',(-1.70562212620408,-0.407041111792943,
-0.0717778861362652));
#20020=CARTESIAN_POINT('Ctrl Pts',(-1.70107730356824,-0.387888272594439,
-0.143648558862931));
#20021=CARTESIAN_POINT('Ctrl Pts',(-1.69769003172132,-0.373243761060365,
-0.178166559972324));
#20022=CARTESIAN_POINT('Ctrl Pts',(-1.68958170688653,-0.335108247315849,
-0.244262842368623));
#20023=CARTESIAN_POINT('Ctrl Pts',(-1.68332504372461,-0.303141259068212,
-0.283214707341173));
#20024=CARTESIAN_POINT('Ctrl Pts',(-1.67246562047521,-0.236152929235938,
-0.341837165343982));
#20025=CARTESIAN_POINT('Ctrl Pts',(-1.66658649961961,-0.192480977588836,
-0.368536561654407));
#20026=CARTESIAN_POINT('Ctrl Pts',(-1.66063136041479,-0.123823518623745,
-0.394174530911059));
#20027=CARTESIAN_POINT('Ctrl Pts',(-1.65912839404491,-0.101649918886749,
-0.400393769631748));
#20028=CARTESIAN_POINT('Ctrl Pts',(-1.65807299932179,-0.0793800000000001,
-0.404717578595296));
#20029=CARTESIAN_POINT('',(-1.45861320581289,-0.07938,-0.886256117232623));
#20030=CARTESIAN_POINT('Origin',(0.,-0.07938,0.));
#20031=CARTESIAN_POINT('',(-0.886256117232623,-0.07938,-1.45861320581289));
#20032=CARTESIAN_POINT('Ctrl Pts',(-1.45861320581289,-0.0793800000000001,
-0.886256117232623));
#20033=CARTESIAN_POINT('Ctrl Pts',(-1.45630208793976,-0.101649918886749,
-0.890059788636852));
#20034=CARTESIAN_POINT('Ctrl Pts',(-1.45296717977858,-0.123823518623745,
-0.895520212222106));
#20035=CARTESIAN_POINT('Ctrl Pts',(-1.43904931717599,-0.192480977588835,
-0.917859913453974));
#20036=CARTESIAN_POINT('Ctrl Pts',(-1.4243271592157,-0.236152929235937,
-0.940896403863072));
#20037=CARTESIAN_POINT('Ctrl Pts',(-1.39055359345152,-0.303141259068212,
-0.990027513266106));
#20038=CARTESIAN_POINT('Ctrl Pts',(-1.36743459453896,-0.335108247315849,
-1.02199477007745));
#20039=CARTESIAN_POINT('Ctrl Pts',(-1.32643091652006,-0.373243761060364,
-1.07446535104584));
#20040=CARTESIAN_POINT('Ctrl Pts',(-1.30441816675528,-0.387888272594439,
-1.10126842659597));
#20041=CARTESIAN_POINT('Ctrl Pts',(-1.25681160160691,-0.407041111792943,
-1.15530234155453));
#20042=CARTESIAN_POINT('Ctrl Pts',(-1.23119764287622,-0.411552957311693,
-1.18251418313119));
#20043=CARTESIAN_POINT('Ctrl Pts',(-1.18251418313119,-0.411552957311693,
-1.23119764287622));
#20044=CARTESIAN_POINT('Ctrl Pts',(-1.15530234155453,-0.407041111792943,
-1.25681160160691));
#20045=CARTESIAN_POINT('Ctrl Pts',(-1.10126842659597,-0.387888272594439,
-1.30441816675528));
#20046=CARTESIAN_POINT('Ctrl Pts',(-1.07446535104584,-0.373243761060364,
-1.32643091652006));
#20047=CARTESIAN_POINT('Ctrl Pts',(-1.02199477007745,-0.335108247315848,
-1.36743459453896));
#20048=CARTESIAN_POINT('Ctrl Pts',(-0.990027513266105,-0.303141259068211,
-1.39055359345152));
#20049=CARTESIAN_POINT('Ctrl Pts',(-0.940896403863071,-0.236152929235936,
-1.42432715921571));
#20050=CARTESIAN_POINT('Ctrl Pts',(-0.917859913453974,-0.192480977588835,
-1.43904931717599));
#20051=CARTESIAN_POINT('Ctrl Pts',(-0.895520212222106,-0.123823518623745,
-1.45296717977858));
#20052=CARTESIAN_POINT('Ctrl Pts',(-0.890059788636851,-0.101649918886749,
-1.45630208793976));
#20053=CARTESIAN_POINT('Ctrl Pts',(-0.886256117232623,-0.0793800000000001,
-1.45861320581289));
#20054=CARTESIAN_POINT('',(-0.404717578595295,-0.07938,-1.65807299932179));
#20055=CARTESIAN_POINT('Origin',(0.,-0.07938,0.));
#20056=CARTESIAN_POINT('',(0.404717578595296,-0.07938,-1.65807299932179));
#20057=CARTESIAN_POINT('Ctrl Pts',(-0.404717578595296,-0.0793800000000001,
-1.65807299932179));
#20058=CARTESIAN_POINT('Ctrl Pts',(-0.400393769631747,-0.101649918886749,
-1.65912839404491));
#20059=CARTESIAN_POINT('Ctrl Pts',(-0.394174530911058,-0.123823518623746,
-1.66063136041479));
#20060=CARTESIAN_POINT('Ctrl Pts',(-0.368536561654407,-0.192480977588836,
-1.66658649961961));
#20061=CARTESIAN_POINT('Ctrl Pts',(-0.341837165343982,-0.236152929235938,
-1.67246562047521));
#20062=CARTESIAN_POINT('Ctrl Pts',(-0.283214707341173,-0.303141259068212,
-1.68332504372461));
#20063=CARTESIAN_POINT('Ctrl Pts',(-0.244262842368623,-0.335108247315849,
-1.68958170688653));
#20064=CARTESIAN_POINT('Ctrl Pts',(-0.178166559972324,-0.373243761060364,
-1.69769003172132));
#20065=CARTESIAN_POINT('Ctrl Pts',(-0.143648558862931,-0.387888272594439,
-1.70107730356824));
#20066=CARTESIAN_POINT('Ctrl Pts',(-0.0717778861362653,-0.407041111792943,
-1.70562212620408));
#20067=CARTESIAN_POINT('Ctrl Pts',(-0.034424404517331,-0.411552957311693,
-1.706752));
#20068=CARTESIAN_POINT('Ctrl Pts',(0.0344244045173312,-0.411552957311693,
-1.706752));
#20069=CARTESIAN_POINT('Ctrl Pts',(0.0717778861362655,-0.407041111792943,
-1.70562212620408));
#20070=CARTESIAN_POINT('Ctrl Pts',(0.143648558862931,-0.387888272594439,
-1.70107730356824));
#20071=CARTESIAN_POINT('Ctrl Pts',(0.178166559972324,-0.373243761060364,
-1.69769003172132));
#20072=CARTESIAN_POINT('Ctrl Pts',(0.244262842368623,-0.335108247315849,
-1.68958170688653));
#20073=CARTESIAN_POINT('Ctrl Pts',(0.283214707341173,-0.303141259068212,
-1.68332504372461));
#20074=CARTESIAN_POINT('Ctrl Pts',(0.341837165343982,-0.236152929235937,
-1.67246562047521));
#20075=CARTESIAN_POINT('Ctrl Pts',(0.368536561654407,-0.192480977588835,
-1.66658649961961));
#20076=CARTESIAN_POINT('Ctrl Pts',(0.394174530911059,-0.123823518623745,
-1.66063136041479));
#20077=CARTESIAN_POINT('Ctrl Pts',(0.400393769631748,-0.101649918886749,
-1.65912839404491));
#20078=CARTESIAN_POINT('Ctrl Pts',(0.404717578595296,-0.0793800000000001,
-1.65807299932179));
#20079=CARTESIAN_POINT('',(0.886256117232623,-0.07938,-1.45861320581289));
#20080=CARTESIAN_POINT('Origin',(0.,-0.07938,0.));
#20081=CARTESIAN_POINT('',(1.45861320581289,-0.07938,-0.886256117232623));
#20082=CARTESIAN_POINT('Ctrl Pts',(0.886256117232623,-0.0793800000000001,
-1.45861320581289));
#20083=CARTESIAN_POINT('Ctrl Pts',(0.890059788636852,-0.101649918886749,
-1.45630208793976));
#20084=CARTESIAN_POINT('Ctrl Pts',(0.895520212222106,-0.123823518623745,
-1.45296717977858));
#20085=CARTESIAN_POINT('Ctrl Pts',(0.917859913453974,-0.192480977588835,
-1.43904931717599));
#20086=CARTESIAN_POINT('Ctrl Pts',(0.940896403863072,-0.236152929235937,
-1.4243271592157));
#20087=CARTESIAN_POINT('Ctrl Pts',(0.990027513266106,-0.303141259068211,
-1.39055359345152));
#20088=CARTESIAN_POINT('Ctrl Pts',(1.02199477007745,-0.335108247315849,
-1.36743459453896));
#20089=CARTESIAN_POINT('Ctrl Pts',(1.07446535104584,-0.373243761060364,
-1.32643091652006));
#20090=CARTESIAN_POINT('Ctrl Pts',(1.10126842659597,-0.387888272594439,
-1.30441816675528));
#20091=CARTESIAN_POINT('Ctrl Pts',(1.15530234155453,-0.407041111792943,
-1.25681160160691));
#20092=CARTESIAN_POINT('Ctrl Pts',(1.18251418313119,-0.411552957311693,
-1.23119764287622));
#20093=CARTESIAN_POINT('Ctrl Pts',(1.23119764287622,-0.411552957311693,
-1.18251418313119));
#20094=CARTESIAN_POINT('Ctrl Pts',(1.25681160160691,-0.407041111792943,
-1.15530234155453));
#20095=CARTESIAN_POINT('Ctrl Pts',(1.30441816675528,-0.387888272594439,
-1.10126842659597));
#20096=CARTESIAN_POINT('Ctrl Pts',(1.32643091652006,-0.373243761060364,
-1.07446535104584));
#20097=CARTESIAN_POINT('Ctrl Pts',(1.36743459453896,-0.335108247315849,
-1.02199477007745));
#20098=CARTESIAN_POINT('Ctrl Pts',(1.39055359345152,-0.303141259068212,
-0.990027513266105));
#20099=CARTESIAN_POINT('Ctrl Pts',(1.4243271592157,-0.236152929235937,-0.940896403863071));
#20100=CARTESIAN_POINT('Ctrl Pts',(1.43904931717599,-0.192480977588835,
-0.917859913453974));
#20101=CARTESIAN_POINT('Ctrl Pts',(1.45296717977858,-0.123823518623745,
-0.895520212222106));
#20102=CARTESIAN_POINT('Ctrl Pts',(1.45630208793976,-0.101649918886749,
-0.890059788636852));
#20103=CARTESIAN_POINT('Ctrl Pts',(1.45861320581289,-0.0793800000000001,
-0.886256117232623));
#20104=CARTESIAN_POINT('',(1.65807299932179,-0.07938,-0.404717578595296));
#20105=CARTESIAN_POINT('Origin',(0.,-0.07938,0.));
#20106=CARTESIAN_POINT('',(1.65807299932179,-0.07938,0.404717578595296));
#20107=CARTESIAN_POINT('Ctrl Pts',(1.65807299932179,-0.0793800000000001,
-0.404717578595296));
#20108=CARTESIAN_POINT('Ctrl Pts',(1.65912839404491,-0.101649918886749,
-0.400393769631747));
#20109=CARTESIAN_POINT('Ctrl Pts',(1.66063136041479,-0.123823518623745,
-0.394174530911058));
#20110=CARTESIAN_POINT('Ctrl Pts',(1.66658649961961,-0.192480977588835,
-0.368536561654407));
#20111=CARTESIAN_POINT('Ctrl Pts',(1.67246562047521,-0.236152929235937,
-0.341837165343982));
#20112=CARTESIAN_POINT('Ctrl Pts',(1.68332504372461,-0.303141259068212,
-0.283214707341173));
#20113=CARTESIAN_POINT('Ctrl Pts',(1.68958170688653,-0.335108247315849,
-0.244262842368623));
#20114=CARTESIAN_POINT('Ctrl Pts',(1.69769003172132,-0.373243761060364,
-0.178166559972324));
#20115=CARTESIAN_POINT('Ctrl Pts',(1.70107730356824,-0.387888272594439,
-0.143648558862931));
#20116=CARTESIAN_POINT('Ctrl Pts',(1.70562212620408,-0.407041111792943,
-0.0717778861362655));
#20117=CARTESIAN_POINT('Ctrl Pts',(1.706752,-0.411552957311693,-0.0344244045173312));
#20118=CARTESIAN_POINT('Ctrl Pts',(1.706752,-0.411552957311693,0.0344244045173312));
#20119=CARTESIAN_POINT('Ctrl Pts',(1.70562212620408,-0.407041111792943,
0.0717778861362655));
#20120=CARTESIAN_POINT('Ctrl Pts',(1.70107730356824,-0.387888272594439,
0.143648558862931));
#20121=CARTESIAN_POINT('Ctrl Pts',(1.69769003172132,-0.373243761060364,
0.178166559972324));
#20122=CARTESIAN_POINT('Ctrl Pts',(1.68958170688653,-0.335108247315849,
0.244262842368623));
#20123=CARTESIAN_POINT('Ctrl Pts',(1.68332504372461,-0.303141259068212,
0.283214707341173));
#20124=CARTESIAN_POINT('Ctrl Pts',(1.67246562047521,-0.236152929235937,
0.341837165343982));
#20125=CARTESIAN_POINT('Ctrl Pts',(1.66658649961961,-0.192480977588835,
0.368536561654407));
#20126=CARTESIAN_POINT('Ctrl Pts',(1.66063136041479,-0.123823518623745,
0.394174530911058));
#20127=CARTESIAN_POINT('Ctrl Pts',(1.65912839404491,-0.101649918886749,
0.400393769631747));
#20128=CARTESIAN_POINT('Ctrl Pts',(1.65807299932179,-0.0793800000000001,
0.404717578595296));
#20129=CARTESIAN_POINT('Origin',(0.,-0.07938,0.));
#20130=CARTESIAN_POINT('Origin',(0.,-0.07938,0.));
#20131=CARTESIAN_POINT('',(0.397005914195118,-0.07938,1.59456899932179));
#20132=CARTESIAN_POINT('Origin',(0.,-0.07938,0.));
#20133=CARTESIAN_POINT('Origin',(-3.33066907387547E-16,-0.07938,1.675));
#20134=CARTESIAN_POINT('Origin',(-3.33066907387547E-16,0.,1.675));
#20135=CARTESIAN_POINT('',(-0.397005914195118,-0.07938,1.59456899932179));
#20136=CARTESIAN_POINT('Ctrl Pts',(-0.397005914195119,-0.0793800000000001,
1.59456899932179));
#20137=CARTESIAN_POINT('Ctrl Pts',(-0.3886265584581,-0.123401821157026,
1.59665523941937));
#20138=CARTESIAN_POINT('Ctrl Pts',(-0.373030350867485,-0.166543350814306,
1.60050712143809));
#20139=CARTESIAN_POINT('Ctrl Pts',(-0.333298652394954,-0.237231147975234,
1.60919314384089));
#20140=CARTESIAN_POINT('Ctrl Pts',(-0.311480544243687,-0.266264900654909,
1.61365775139403));
#20141=CARTESIAN_POINT('Ctrl Pts',(-0.261368388670537,-0.317195968905306,
1.62252828437015));
#20142=CARTESIAN_POINT('Ctrl Pts',(-0.233069203882014,-0.33909093068465,
1.62691869420078));
#20143=CARTESIAN_POINT('Ctrl Pts',(-0.174042761838764,-0.373586846396559,
1.63426473152765));
#20144=CARTESIAN_POINT('Ctrl Pts',(-0.14036578147155,-0.388086240756494,
1.63761964365402));
#20145=CARTESIAN_POINT('Ctrl Pts',(-0.0701778381840615,-0.407068917407805,
1.64212536811722));
#20146=CARTESIAN_POINT('Ctrl Pts',(-0.0336652739555918,-0.411552957311693,
1.643248));
#20147=CARTESIAN_POINT('Ctrl Pts',(0.0336652739555913,-0.411552957311693,
1.643248));
#20148=CARTESIAN_POINT('Ctrl Pts',(0.070177838184061,-0.407068917407805,
1.64212536811722));
#20149=CARTESIAN_POINT('Ctrl Pts',(0.140365781471549,-0.388086240756494,
1.63761964365402));
#20150=CARTESIAN_POINT('Ctrl Pts',(0.174042761838763,-0.373586846396559,
1.63426473152765));
#20151=CARTESIAN_POINT('Ctrl Pts',(0.233069203882014,-0.33909093068465,
1.62691869420078));
#20152=CARTESIAN_POINT('Ctrl Pts',(0.261368388670536,-0.317195968905306,
1.62252828437015));
#20153=CARTESIAN_POINT('Ctrl Pts',(0.311480544243686,-0.266264900654908,
1.61365775139403));
#20154=CARTESIAN_POINT('Ctrl Pts',(0.333298652394954,-0.237231147975234,
1.60919314384089));
#20155=CARTESIAN_POINT('Ctrl Pts',(0.373030350867484,-0.166543350814306,
1.60050712143809));
#20156=CARTESIAN_POINT('Ctrl Pts',(0.388626558458099,-0.123401821157026,
1.59665523941937));
#20157=CARTESIAN_POINT('Ctrl Pts',(0.397005914195118,-0.07938,1.59456899932179));
#20158=CARTESIAN_POINT('Origin',(-3.33066907387547E-16,-0.07938,1.675));
#20159=CARTESIAN_POINT('Origin',(0.,-0.07938,0.));
#20160=CARTESIAN_POINT('',(-0.846804978391754,-0.07938,1.40825612658882));
#20161=CARTESIAN_POINT('Origin',(0.,-0.07938,0.));
#20162=CARTESIAN_POINT('Origin',(-1.18440385848747,-0.07938,1.18440385848747));
#20163=CARTESIAN_POINT('Origin',(-1.18440385848747,0.,1.18440385848747));
#20164=CARTESIAN_POINT('',(-1.40825612658882,-0.07938,0.846804978391753));
#20165=CARTESIAN_POINT('Ctrl Pts',(-1.40825612658882,-0.0793800000000001,
0.846804978391753));
#20166=CARTESIAN_POINT('Ctrl Pts',(-1.40380622184538,-0.123401821157026,
0.854205272175555));
#20167=CARTESIAN_POINT('Ctrl Pts',(-1.39550172959303,-0.166543350814306,
0.867957148219442));
#20168=CARTESIAN_POINT('Ctrl Pts',(-1.3735491215176,-0.237231147975235,
0.902193646979983));
#20169=CARTESIAN_POINT('Ctrl Pts',(-1.36127834356734,-0.266264900654909,
0.920778333482565));
#20170=CARTESIAN_POINT('Ctrl Pts',(-1.33211611256184,-0.317195968905306,
0.962485392528369));
#20171=CARTESIAN_POINT('Ctrl Pts',(-1.31521005565926,-0.339090930684651,
0.985600426557816));
#20172=CARTESIAN_POINT('Ctrl Pts',(-1.27866649102984,-0.373586846396559,
1.03253285680459));
#20173=CARTESIAN_POINT('Ctrl Pts',(-1.25722555095714,-0.388086240756494,
1.05871835910697));
#20174=CARTESIAN_POINT('Ctrl Pts',(-1.2107812086231,-0.407068917407805,
1.11153475808518));
#20175=CARTESIAN_POINT('Ctrl Pts',(-1.18575674747573,-0.411552957311693,
1.13814686046673));
#20176=CARTESIAN_POINT('Ctrl Pts',(-1.13814686046673,-0.411552957311693,
1.18575674747573));
#20177=CARTESIAN_POINT('Ctrl Pts',(-1.11153475808518,-0.407068917407805,
1.2107812086231));
#20178=CARTESIAN_POINT('Ctrl Pts',(-1.05871835910697,-0.388086240756494,
1.25722555095714));
#20179=CARTESIAN_POINT('Ctrl Pts',(-1.03253285680459,-0.373586846396559,
1.27866649102984));
#20180=CARTESIAN_POINT('Ctrl Pts',(-0.985600426557816,-0.33909093068465,
1.31521005565926));
#20181=CARTESIAN_POINT('Ctrl Pts',(-0.962485392528369,-0.317195968905306,
1.33211611256184));
#20182=CARTESIAN_POINT('Ctrl Pts',(-0.920778333482565,-0.266264900654908,
1.36127834356734));
#20183=CARTESIAN_POINT('Ctrl Pts',(-0.902193646979983,-0.237231147975234,
1.3735491215176));
#20184=CARTESIAN_POINT('Ctrl Pts',(-0.867957148219442,-0.166543350814306,
1.39550172959303));
#20185=CARTESIAN_POINT('Ctrl Pts',(-0.854205272175555,-0.123401821157026,
1.40380622184538));
#20186=CARTESIAN_POINT('Ctrl Pts',(-0.846804978391753,-0.0793800000000001,
1.40825612658882));
#20187=CARTESIAN_POINT('Origin',(-1.18440385848747,-0.07938,1.18440385848747));
#20188=CARTESIAN_POINT('Origin',(0.,-0.07938,0.));
#20189=CARTESIAN_POINT('',(-1.59456899932179,-0.07938,0.397005914195118));
#20190=CARTESIAN_POINT('Origin',(0.,-0.07938,0.));
#20191=CARTESIAN_POINT('Origin',(-1.675,-0.07938,-2.22044604925031E-16));
#20192=CARTESIAN_POINT('Origin',(-1.675,0.,-2.22044604925031E-16));
#20193=CARTESIAN_POINT('',(-1.59456899932179,-0.07938,-0.397005914195118));
#20194=CARTESIAN_POINT('',(-1.643248,-0.411552957311693,3.47540551556327E-18));
#20195=CARTESIAN_POINT('Ctrl Pts',(-1.59456899932179,-0.0793800000000001,
-0.397005914195119));
#20196=CARTESIAN_POINT('Ctrl Pts',(-1.59665523941937,-0.123401821157026,
-0.388626558458099));
#20197=CARTESIAN_POINT('Ctrl Pts',(-1.60050712143809,-0.166543350814306,
-0.373030350867485));
#20198=CARTESIAN_POINT('Ctrl Pts',(-1.60919314384089,-0.237231147975234,
-0.333298652394954));
#20199=CARTESIAN_POINT('Ctrl Pts',(-1.61365775139403,-0.266264900654909,
-0.311480544243686));
#20200=CARTESIAN_POINT('Ctrl Pts',(-1.62252828437015,-0.317195968905306,
-0.261368388670537));
#20201=CARTESIAN_POINT('Ctrl Pts',(-1.62691869420078,-0.33909093068465,
-0.233069203882014));
#20202=CARTESIAN_POINT('Ctrl Pts',(-1.63426473152765,-0.373586846396559,
-0.174042761838764));
#20203=CARTESIAN_POINT('Ctrl Pts',(-1.63761964365402,-0.388086240756494,
-0.140365781471549));
#20204=CARTESIAN_POINT('Ctrl Pts',(-1.64212536811722,-0.407068917407805,
-0.0701778381840614));
#20205=CARTESIAN_POINT('Ctrl Pts',(-1.643248,-0.411552957311693,-0.0336652739555917));
#20206=CARTESIAN_POINT('Ctrl Pts',(-1.643248,-0.411552957311693,-2.0122792321331E-16));
#20207=CARTESIAN_POINT('Origin',(-1.675,-0.07938,-2.22044604925031E-16));
#20208=CARTESIAN_POINT('Ctrl Pts',(-1.643248,-0.411552957311693,-1.94289029309402E-16));
#20209=CARTESIAN_POINT('Ctrl Pts',(-1.643248,-0.411552957311693,0.0336652739555913));
#20210=CARTESIAN_POINT('Ctrl Pts',(-1.64212536811722,-0.407068917407805,
0.0701778381840609));
#20211=CARTESIAN_POINT('Ctrl Pts',(-1.63761964365402,-0.388086240756494,
0.140365781471549));
#20212=CARTESIAN_POINT('Ctrl Pts',(-1.63426473152765,-0.373586846396559,
0.174042761838763));
#20213=CARTESIAN_POINT('Ctrl Pts',(-1.62691869420078,-0.33909093068465,
0.233069203882014));
#20214=CARTESIAN_POINT('Ctrl Pts',(-1.62252828437015,-0.317195968905306,
0.261368388670536));
#20215=CARTESIAN_POINT('Ctrl Pts',(-1.61365775139403,-0.266264900654909,
0.311480544243686));
#20216=CARTESIAN_POINT('Ctrl Pts',(-1.60919314384089,-0.237231147975235,
0.333298652394954));
#20217=CARTESIAN_POINT('Ctrl Pts',(-1.60050712143809,-0.166543350814306,
0.373030350867484));
#20218=CARTESIAN_POINT('Ctrl Pts',(-1.59665523941937,-0.123401821157026,
0.388626558458099));
#20219=CARTESIAN_POINT('Ctrl Pts',(-1.59456899932179,-0.0793800000000001,
0.397005914195118));
#20220=CARTESIAN_POINT('Origin',(0.,-0.07938,0.));
#20221=CARTESIAN_POINT('',(-1.40825612658882,-0.07938,-0.846804978391753));
#20222=CARTESIAN_POINT('Origin',(0.,-0.07938,0.));
#20223=CARTESIAN_POINT('Origin',(-1.18440385848747,-0.07938,-1.18440385848747));
#20224=CARTESIAN_POINT('Origin',(-1.18440385848747,0.,-1.18440385848747));
#20225=CARTESIAN_POINT('',(-0.846804978391753,-0.07938,-1.40825612658882));
#20226=CARTESIAN_POINT('Ctrl Pts',(-0.846804978391753,-0.0793800000000001,
-1.40825612658882));
#20227=CARTESIAN_POINT('Ctrl Pts',(-0.854205272175555,-0.123401821157026,
-1.40380622184538));
#20228=CARTESIAN_POINT('Ctrl Pts',(-0.867957148219442,-0.166543350814306,
-1.39550172959303));
#20229=CARTESIAN_POINT('Ctrl Pts',(-0.902193646979982,-0.237231147975234,
-1.3735491215176));
#20230=CARTESIAN_POINT('Ctrl Pts',(-0.920778333482564,-0.266264900654908,
-1.36127834356734));
#20231=CARTESIAN_POINT('Ctrl Pts',(-0.962485392528368,-0.317195968905306,
-1.33211611256184));
#20232=CARTESIAN_POINT('Ctrl Pts',(-0.985600426557816,-0.33909093068465,
-1.31521005565926));
#20233=CARTESIAN_POINT('Ctrl Pts',(-1.03253285680459,-0.373586846396559,
-1.27866649102984));
#20234=CARTESIAN_POINT('Ctrl Pts',(-1.05871835910697,-0.388086240756494,
-1.25722555095714));
#20235=CARTESIAN_POINT('Ctrl Pts',(-1.11153475808518,-0.407068917407805,
-1.2107812086231));
#20236=CARTESIAN_POINT('Ctrl Pts',(-1.13814686046673,-0.411552957311693,
-1.18575674747573));
#20237=CARTESIAN_POINT('Ctrl Pts',(-1.18575674747573,-0.411552957311693,
-1.13814686046673));
#20238=CARTESIAN_POINT('Ctrl Pts',(-1.2107812086231,-0.407068917407805,
-1.11153475808518));
#20239=CARTESIAN_POINT('Ctrl Pts',(-1.25722555095714,-0.388086240756494,
-1.05871835910697));
#20240=CARTESIAN_POINT('Ctrl Pts',(-1.27866649102984,-0.373586846396559,
-1.03253285680459));
#20241=CARTESIAN_POINT('Ctrl Pts',(-1.31521005565926,-0.33909093068465,
-0.985600426557816));
#20242=CARTESIAN_POINT('Ctrl Pts',(-1.33211611256184,-0.317195968905306,
-0.962485392528369));
#20243=CARTESIAN_POINT('Ctrl Pts',(-1.36127834356734,-0.266264900654909,
-0.920778333482565));
#20244=CARTESIAN_POINT('Ctrl Pts',(-1.3735491215176,-0.237231147975234,
-0.902193646979983));
#20245=CARTESIAN_POINT('Ctrl Pts',(-1.39550172959303,-0.166543350814306,
-0.867957148219442));
#20246=CARTESIAN_POINT('Ctrl Pts',(-1.40380622184538,-0.123401821157026,
-0.854205272175555));
#20247=CARTESIAN_POINT('Ctrl Pts',(-1.40825612658882,-0.07938,-0.846804978391753));
#20248=CARTESIAN_POINT('Origin',(-1.18440385848747,-0.07938,-1.18440385848747));
#20249=CARTESIAN_POINT('Origin',(0.,-0.07938,0.));
#20250=CARTESIAN_POINT('',(-0.397005914195118,-0.07938,-1.59456899932179));
#20251=CARTESIAN_POINT('Origin',(0.,-0.07938,0.));
#20252=CARTESIAN_POINT('Origin',(1.11022302462516E-16,-0.07938,-1.675));
#20253=CARTESIAN_POINT('Origin',(1.11022302462516E-16,0.,-1.675));
#20254=CARTESIAN_POINT('',(0.397005914195118,-0.07938,-1.59456899932179));
#20255=CARTESIAN_POINT('Ctrl Pts',(0.397005914195119,-0.0793800000000001,
-1.59456899932179));
#20256=CARTESIAN_POINT('Ctrl Pts',(0.388626558458099,-0.123401821157026,
-1.59665523941937));
#20257=CARTESIAN_POINT('Ctrl Pts',(0.373030350867485,-0.166543350814306,
-1.60050712143809));
#20258=CARTESIAN_POINT('Ctrl Pts',(0.333298652394954,-0.237231147975234,
-1.60919314384089));
#20259=CARTESIAN_POINT('Ctrl Pts',(0.311480544243686,-0.266264900654909,
-1.61365775139403));
#20260=CARTESIAN_POINT('Ctrl Pts',(0.261368388670537,-0.317195968905306,
-1.62252828437015));
#20261=CARTESIAN_POINT('Ctrl Pts',(0.233069203882014,-0.33909093068465,
-1.62691869420078));
#20262=CARTESIAN_POINT('Ctrl Pts',(0.174042761838763,-0.373586846396559,
-1.63426473152765));
#20263=CARTESIAN_POINT('Ctrl Pts',(0.140365781471549,-0.388086240756494,
-1.63761964365402));
#20264=CARTESIAN_POINT('Ctrl Pts',(0.0701778381840612,-0.407068917407805,
-1.64212536811722));
#20265=CARTESIAN_POINT('Ctrl Pts',(0.0336652739555916,-0.411552957311693,
-1.643248));
#20266=CARTESIAN_POINT('Ctrl Pts',(-0.0336652739555915,-0.411552957311693,
-1.643248));
#20267=CARTESIAN_POINT('Ctrl Pts',(-0.0701778381840612,-0.407068917407805,
-1.64212536811722));
#20268=CARTESIAN_POINT('Ctrl Pts',(-0.140365781471549,-0.388086240756494,
-1.63761964365402));
#20269=CARTESIAN_POINT('Ctrl Pts',(-0.174042761838764,-0.373586846396559,
-1.63426473152765));
#20270=CARTESIAN_POINT('Ctrl Pts',(-0.233069203882014,-0.33909093068465,
-1.62691869420078));
#20271=CARTESIAN_POINT('Ctrl Pts',(-0.261368388670536,-0.317195968905306,
-1.62252828437015));
#20272=CARTESIAN_POINT('Ctrl Pts',(-0.311480544243686,-0.266264900654908,
-1.61365775139403));
#20273=CARTESIAN_POINT('Ctrl Pts',(-0.333298652394954,-0.237231147975234,
-1.60919314384089));
#20274=CARTESIAN_POINT('Ctrl Pts',(-0.373030350867485,-0.166543350814306,
-1.60050712143809));
#20275=CARTESIAN_POINT('Ctrl Pts',(-0.388626558458099,-0.123401821157026,
-1.59665523941937));
#20276=CARTESIAN_POINT('Ctrl Pts',(-0.397005914195118,-0.07938,-1.59456899932179));
#20277=CARTESIAN_POINT('Origin',(1.11022302462516E-16,-0.07938,-1.675));
#20278=CARTESIAN_POINT('Origin',(0.,-0.07938,0.));
#20279=CARTESIAN_POINT('',(0.846804978391753,-0.07938,-1.40825612658882));
#20280=CARTESIAN_POINT('Origin',(0.,-0.07938,0.));
#20281=CARTESIAN_POINT('Origin',(1.18440385848747,-0.07938,-1.18440385848747));
#20282=CARTESIAN_POINT('Origin',(1.18440385848747,0.,-1.18440385848747));
#20283=CARTESIAN_POINT('',(1.40825612658882,-0.07938,-0.846804978391753));
#20284=CARTESIAN_POINT('Ctrl Pts',(1.40825612658882,-0.0793800000000001,
-0.846804978391753));
#20285=CARTESIAN_POINT('Ctrl Pts',(1.40380622184538,-0.123401821157026,
-0.854205272175555));
#20286=CARTESIAN_POINT('Ctrl Pts',(1.39550172959303,-0.166543350814306,
-0.867957148219442));
#20287=CARTESIAN_POINT('Ctrl Pts',(1.3735491215176,-0.237231147975234,-0.902193646979983));
#20288=CARTESIAN_POINT('Ctrl Pts',(1.36127834356734,-0.266264900654908,
-0.920778333482565));
#20289=CARTESIAN_POINT('Ctrl Pts',(1.33211611256184,-0.317195968905306,
-0.962485392528369));
#20290=CARTESIAN_POINT('Ctrl Pts',(1.31521005565926,-0.33909093068465,-0.985600426557816));
#20291=CARTESIAN_POINT('Ctrl Pts',(1.27866649102984,-0.373586846396559,
-1.03253285680459));
#20292=CARTESIAN_POINT('Ctrl Pts',(1.25722555095714,-0.388086240756494,
-1.05871835910697));
#20293=CARTESIAN_POINT('Ctrl Pts',(1.2107812086231,-0.407068917407805,-1.11153475808518));
#20294=CARTESIAN_POINT('Ctrl Pts',(1.18575674747573,-0.411552957311693,
-1.13814686046673));
#20295=CARTESIAN_POINT('Ctrl Pts',(1.13814686046673,-0.411552957311693,
-1.18575674747573));
#20296=CARTESIAN_POINT('Ctrl Pts',(1.11153475808518,-0.407068917407805,
-1.2107812086231));
#20297=CARTESIAN_POINT('Ctrl Pts',(1.05871835910697,-0.388086240756494,
-1.25722555095714));
#20298=CARTESIAN_POINT('Ctrl Pts',(1.03253285680459,-0.373586846396559,
-1.27866649102984));
#20299=CARTESIAN_POINT('Ctrl Pts',(0.985600426557816,-0.33909093068465,
-1.31521005565926));
#20300=CARTESIAN_POINT('Ctrl Pts',(0.962485392528369,-0.317195968905306,
-1.33211611256184));
#20301=CARTESIAN_POINT('Ctrl Pts',(0.920778333482565,-0.266264900654909,
-1.36127834356734));
#20302=CARTESIAN_POINT('Ctrl Pts',(0.902193646979983,-0.237231147975234,
-1.3735491215176));
#20303=CARTESIAN_POINT('Ctrl Pts',(0.867957148219442,-0.166543350814306,
-1.39550172959303));
#20304=CARTESIAN_POINT('Ctrl Pts',(0.854205272175555,-0.123401821157026,
-1.40380622184538));
#20305=CARTESIAN_POINT('Ctrl Pts',(0.846804978391753,-0.0793800000000001,
-1.40825612658882));
#20306=CARTESIAN_POINT('Origin',(1.18440385848747,-0.07938,-1.18440385848747));
#20307=CARTESIAN_POINT('Origin',(0.,-0.27783,0.));
#20308=CARTESIAN_POINT('',(-1.643248,-0.47628,2.01239840340529E-16));
#20309=CARTESIAN_POINT('Origin',(0.,-0.47628,0.));
#20310=CARTESIAN_POINT('',(-1.643248,-0.27783,2.01239840340529E-16));
#20311=CARTESIAN_POINT('',(1.59456899932179,-0.07938,0.397005914195118));
#20312=CARTESIAN_POINT('Origin',(0.,-0.07938,0.));
#20313=CARTESIAN_POINT('',(1.59456899932179,-0.07938,-0.397005914195118));
#20314=CARTESIAN_POINT('Ctrl Pts',(1.59456899932179,-0.0793800000000001,
0.397005914195118));
#20315=CARTESIAN_POINT('Ctrl Pts',(1.59665523941937,-0.123401821157026,
0.388626558458099));
#20316=CARTESIAN_POINT('Ctrl Pts',(1.60050712143809,-0.166543350814306,
0.373030350867485));
#20317=CARTESIAN_POINT('Ctrl Pts',(1.60919314384089,-0.237231147975234,
0.333298652394954));
#20318=CARTESIAN_POINT('Ctrl Pts',(1.61365775139403,-0.266264900654909,
0.311480544243686));
#20319=CARTESIAN_POINT('Ctrl Pts',(1.62252828437015,-0.317195968905306,
0.261368388670537));
#20320=CARTESIAN_POINT('Ctrl Pts',(1.62691869420078,-0.33909093068465,0.233069203882014));
#20321=CARTESIAN_POINT('Ctrl Pts',(1.63426473152765,-0.373586846396559,
0.174042761838764));
#20322=CARTESIAN_POINT('Ctrl Pts',(1.63761964365402,-0.388086240756494,
0.140365781471549));
#20323=CARTESIAN_POINT('Ctrl Pts',(1.64212536811722,-0.407068917407805,
0.0701778381840612));
#20324=CARTESIAN_POINT('Ctrl Pts',(1.643248,-0.411552957311693,0.0336652739555916));
#20325=CARTESIAN_POINT('Ctrl Pts',(1.643248,-0.411552957311693,-0.0336652739555916));
#20326=CARTESIAN_POINT('Ctrl Pts',(1.64212536811722,-0.407068917407805,
-0.0701778381840612));
#20327=CARTESIAN_POINT('Ctrl Pts',(1.63761964365402,-0.388086240756494,
-0.140365781471549));
#20328=CARTESIAN_POINT('Ctrl Pts',(1.63426473152765,-0.373586846396559,
-0.174042761838764));
#20329=CARTESIAN_POINT('Ctrl Pts',(1.62691869420078,-0.33909093068465,-0.233069203882014));
#20330=CARTESIAN_POINT('Ctrl Pts',(1.62252828437015,-0.317195968905306,
-0.261368388670537));
#20331=CARTESIAN_POINT('Ctrl Pts',(1.61365775139403,-0.266264900654909,
-0.311480544243686));
#20332=CARTESIAN_POINT('Ctrl Pts',(1.60919314384089,-0.237231147975234,
-0.333298652394954));
#20333=CARTESIAN_POINT('Ctrl Pts',(1.60050712143809,-0.166543350814306,
-0.373030350867485));
#20334=CARTESIAN_POINT('Ctrl Pts',(1.59665523941937,-0.123401821157026,
-0.388626558458099));
#20335=CARTESIAN_POINT('Ctrl Pts',(1.59456899932179,-0.07938,-0.397005914195118));
#20336=CARTESIAN_POINT('Origin',(0.,-0.07938,0.));
#20337=CARTESIAN_POINT('Origin',(0.,-0.07938,0.));
#20338=CARTESIAN_POINT('Origin',(1.675,-0.07938,0.));
#20339=CARTESIAN_POINT('Origin',(1.675,0.,0.));
#20340=CARTESIAN_POINT('Origin',(1.675,-0.07938,0.));
#20341=CARTESIAN_POINT('Origin',(0.,-0.47628,0.));
#20342=CARTESIAN_POINT('Origin',(0.,-0.07938,0.));
#20343=CARTESIAN_POINT('',(0.,0.,0.));
#20344=CARTESIAN_POINT('Origin',(1.70469,0.695,0.));
#20345=CARTESIAN_POINT('',(-1.70469,0.695,-2.0876431520385E-16));
#20346=CARTESIAN_POINT('Origin',(0.,0.695,0.));
#20347=CARTESIAN_POINT('',(-1.65031,0.695,-2.02104685910087E-16));
#20348=CARTESIAN_POINT('Origin',(0.,0.695,0.));
#20349=CARTESIAN_POINT('Origin',(0.,0.6575,0.));
#20350=CARTESIAN_POINT('',(-1.70469,0.62,-2.0876431520385E-16));
#20351=CARTESIAN_POINT('Origin',(0.,0.62,0.));
#20352=CARTESIAN_POINT('',(-1.70469,0.6575,-2.0876431520385E-16));
#20353=CARTESIAN_POINT('Origin',(1.65031,0.62,0.));
#20354=CARTESIAN_POINT('',(-1.65031,0.62,-2.02104685910087E-16));
#20355=CARTESIAN_POINT('Origin',(0.,0.62,0.));
#20356=CARTESIAN_POINT('Origin',(0.,0.6575,0.));
#20357=CARTESIAN_POINT('',(-1.65031,0.6575,-2.02104685910087E-16));
#20358=CARTESIAN_POINT('Origin',(1.70469,-0.62,0.));
#20359=CARTESIAN_POINT('',(-1.70469,-0.62,-2.0876431520385E-16));
#20360=CARTESIAN_POINT('Origin',(0.,-0.62,0.));
#20361=CARTESIAN_POINT('',(-1.65031,-0.62,-2.02104685910087E-16));
#20362=CARTESIAN_POINT('Origin',(0.,-0.62,0.));
#20363=CARTESIAN_POINT('Origin',(0.,-0.6575,0.));
#20364=CARTESIAN_POINT('',(-1.70469,-0.695,-2.0876431520385E-16));
#20365=CARTESIAN_POINT('Origin',(0.,-0.695,0.));
#20366=CARTESIAN_POINT('',(-1.70469,-0.6575,-2.0876431520385E-16));
#20367=CARTESIAN_POINT('Origin',(1.65031,-0.695,0.));
#20368=CARTESIAN_POINT('',(-1.65031,-0.695,-2.02104685910087E-16));
#20369=CARTESIAN_POINT('Origin',(0.,-0.695,0.));
#20370=CARTESIAN_POINT('Origin',(0.,-0.6575,0.));
#20371=CARTESIAN_POINT('',(-1.65031,-0.6575,-2.02104685910087E-16));
#20372=CARTESIAN_POINT('',(0.,0.,0.));
#20373=CARTESIAN_POINT('',(0.,0.,0.));
#20374=CARTESIAN_POINT('',(0.,0.,0.));
#20375=CARTESIAN_POINT('',(0.,0.,0.));
#20376=CARTESIAN_POINT('',(0.,0.,0.));
#20377=CARTESIAN_POINT('',(0.,0.,0.));
#20378=CARTESIAN_POINT('Origin',(-0.1,0.82,-0.3));
#20379=CARTESIAN_POINT('',(-1.,0.82,-0.3));
#20380=CARTESIAN_POINT('',(-1.,1.,-0.3));
#20381=CARTESIAN_POINT('',(-1.,0.41,-0.3));
#20382=CARTESIAN_POINT('',(30.,0.82,-0.3));
#20383=CARTESIAN_POINT('',(-0.1,0.82,-0.3));
#20384=CARTESIAN_POINT('',(30.,1.,-0.3));
#20385=CARTESIAN_POINT('',(30.,0.41,-0.3));
#20386=CARTESIAN_POINT('',(-0.05,1.,-0.3));
#20387=CARTESIAN_POINT('Origin',(-0.1,0.82,-0.55));
#20388=CARTESIAN_POINT('',(-1.,0.82,-0.55));
#20389=CARTESIAN_POINT('',(-1.,0.82,-0.275));
#20390=CARTESIAN_POINT('',(30.,0.82,-0.55));
#20391=CARTESIAN_POINT('',(-0.1,0.82,-0.55));
#20392=CARTESIAN_POINT('',(30.,0.82,-0.275));
#20393=CARTESIAN_POINT('Origin',(-0.1,0.67,-0.55));
#20394=CARTESIAN_POINT('',(-1.,0.67,-0.55));
#20395=CARTESIAN_POINT('',(-1.,0.335,-0.55));
#20396=CARTESIAN_POINT('',(30.,0.67,-0.55));
#20397=CARTESIAN_POINT('',(-0.1,0.67,-0.55));
#20398=CARTESIAN_POINT('',(30.,0.335,-0.55));
#20399=CARTESIAN_POINT('Origin',(-0.1,0.42,-0.3));
#20400=CARTESIAN_POINT('',(-1.,0.42,-0.3));
#20401=CARTESIAN_POINT('',(-1.,0.24,-0.12));
#20402=CARTESIAN_POINT('',(30.,0.42,-0.3));
#20403=CARTESIAN_POINT('',(-0.1,0.42,-0.3));
#20404=CARTESIAN_POINT('',(30.,0.24,-0.12));
#20405=CARTESIAN_POINT('Origin',(-0.1,0.42,0.3));
#20406=CARTESIAN_POINT('',(-1.,0.42,0.3));
#20407=CARTESIAN_POINT('',(-1.,0.42,0.15));
#20408=CARTESIAN_POINT('',(30.,0.42,0.3));
#20409=CARTESIAN_POINT('',(-0.1,0.42,0.3));
#20410=CARTESIAN_POINT('',(30.,0.42,0.15));
#20411=CARTESIAN_POINT('Origin',(-0.1,0.67,0.55));
#20412=CARTESIAN_POINT('',(-1.,0.67,0.55));
#20413=CARTESIAN_POINT('',(-1.,0.365,0.245));
#20414=CARTESIAN_POINT('',(30.,0.67,0.55));
#20415=CARTESIAN_POINT('',(-0.1,0.67,0.55));
#20416=CARTESIAN_POINT('',(30.,0.365,0.245));
#20417=CARTESIAN_POINT('Origin',(-0.1,0.82,0.55));
#20418=CARTESIAN_POINT('',(-1.,0.82,0.55));
#20419=CARTESIAN_POINT('',(-1.,0.41,0.55));
#20420=CARTESIAN_POINT('',(30.,0.82,0.55));
#20421=CARTESIAN_POINT('',(-0.1,0.82,0.55));
#20422=CARTESIAN_POINT('',(30.,0.41,0.55));
#20423=CARTESIAN_POINT('Origin',(-0.1,0.82,0.3));
#20424=CARTESIAN_POINT('',(-1.,0.82,0.3));
#20425=CARTESIAN_POINT('',(-1.,0.82,0.15));
#20426=CARTESIAN_POINT('',(30.,0.82,0.3));
#20427=CARTESIAN_POINT('',(-0.1,0.82,0.3));
#20428=CARTESIAN_POINT('',(30.,0.82,0.15));
#20429=CARTESIAN_POINT('Origin',(-0.1,1.05,0.3));
#20430=CARTESIAN_POINT('',(-1.,1.,0.3));
#20431=CARTESIAN_POINT('',(-1.,0.525,0.3));
#20432=CARTESIAN_POINT('',(30.,1.,0.3));
#20433=CARTESIAN_POINT('',(-0.05,1.,0.3));
#20434=CARTESIAN_POINT('',(30.,0.525,0.3));
#20435=CARTESIAN_POINT('Origin',(-0.1,-0.3,-0.82));
#20436=CARTESIAN_POINT('',(-1.,-0.3,-0.82));
#20437=CARTESIAN_POINT('',(-1.,-0.3,-1.));
#20438=CARTESIAN_POINT('',(-1.,-0.3,-0.41));
#20439=CARTESIAN_POINT('',(30.,-0.3,-0.82));
#20440=CARTESIAN_POINT('',(-0.1,-0.3,-0.82));
#20441=CARTESIAN_POINT('',(30.,-0.3,-1.));
#20442=CARTESIAN_POINT('',(30.,-0.3,-0.41));
#20443=CARTESIAN_POINT('',(-0.05,-0.3,-1.));
#20444=CARTESIAN_POINT('Origin',(-0.1,-0.55,-0.82));
#20445=CARTESIAN_POINT('',(-1.,-0.55,-0.82));
#20446=CARTESIAN_POINT('',(-1.,-0.275,-0.82));
#20447=CARTESIAN_POINT('',(30.,-0.55,-0.82));
#20448=CARTESIAN_POINT('',(-0.1,-0.55,-0.82));
#20449=CARTESIAN_POINT('',(30.,-0.275,-0.82));
#20450=CARTESIAN_POINT('Origin',(-0.1,-0.55,-0.67));
#20451=CARTESIAN_POINT('',(-1.,-0.55,-0.67));
#20452=CARTESIAN_POINT('',(-1.,-0.55,-0.335));
#20453=CARTESIAN_POINT('',(30.,-0.55,-0.67));
#20454=CARTESIAN_POINT('',(-0.1,-0.55,-0.67));
#20455=CARTESIAN_POINT('',(30.,-0.55,-0.335));
#20456=CARTESIAN_POINT('Origin',(-0.1,-0.3,-0.42));
#20457=CARTESIAN_POINT('',(-1.,-0.3,-0.42));
#20458=CARTESIAN_POINT('',(-1.,-0.12,-0.24));
#20459=CARTESIAN_POINT('',(30.,-0.3,-0.42));
#20460=CARTESIAN_POINT('',(-0.1,-0.3,-0.42));
#20461=CARTESIAN_POINT('',(30.,-0.12,-0.24));
#20462=CARTESIAN_POINT('Origin',(-0.1,0.3,-0.42));
#20463=CARTESIAN_POINT('',(-1.,0.3,-0.42));
#20464=CARTESIAN_POINT('',(-1.,0.15,-0.42));
#20465=CARTESIAN_POINT('',(30.,0.3,-0.42));
#20466=CARTESIAN_POINT('',(-0.1,0.3,-0.42));
#20467=CARTESIAN_POINT('',(30.,0.15,-0.42));
#20468=CARTESIAN_POINT('Origin',(-0.1,0.55,-0.67));
#20469=CARTESIAN_POINT('',(-1.,0.55,-0.67));
#20470=CARTESIAN_POINT('',(-1.,0.245,-0.365));
#20471=CARTESIAN_POINT('',(30.,0.55,-0.67));
#20472=CARTESIAN_POINT('',(-0.1,0.55,-0.67));
#20473=CARTESIAN_POINT('',(30.,0.245,-0.365));
#20474=CARTESIAN_POINT('Origin',(-0.1,0.55,-0.82));
#20475=CARTESIAN_POINT('',(-1.,0.55,-0.82));
#20476=CARTESIAN_POINT('',(-1.,0.55,-0.41));
#20477=CARTESIAN_POINT('',(30.,0.55,-0.82));
#20478=CARTESIAN_POINT('',(-0.1,0.55,-0.82));
#20479=CARTESIAN_POINT('',(30.,0.55,-0.41));
#20480=CARTESIAN_POINT('Origin',(-0.1,0.3,-0.82));
#20481=CARTESIAN_POINT('',(-1.,0.3,-0.82));
#20482=CARTESIAN_POINT('',(-1.,0.15,-0.82));
#20483=CARTESIAN_POINT('',(30.,0.3,-0.82));
#20484=CARTESIAN_POINT('',(-0.1,0.3,-0.82));
#20485=CARTESIAN_POINT('',(30.,0.15,-0.82));
#20486=CARTESIAN_POINT('Origin',(-0.1,0.3,-1.05));
#20487=CARTESIAN_POINT('',(-1.,0.3,-1.));
#20488=CARTESIAN_POINT('',(-1.,0.3,-0.525));
#20489=CARTESIAN_POINT('',(30.,0.3,-1.));
#20490=CARTESIAN_POINT('',(-0.05,0.3,-1.));
#20491=CARTESIAN_POINT('',(30.,0.3,-0.525));
#20492=CARTESIAN_POINT('Origin',(-0.1,-0.82,0.3));
#20493=CARTESIAN_POINT('',(-1.,-0.82,0.3));
#20494=CARTESIAN_POINT('',(-1.,-1.,0.3));
#20495=CARTESIAN_POINT('',(-1.,-0.41,0.3));
#20496=CARTESIAN_POINT('',(30.,-0.82,0.3));
#20497=CARTESIAN_POINT('',(-0.1,-0.82,0.3));
#20498=CARTESIAN_POINT('',(30.,-1.,0.3));
#20499=CARTESIAN_POINT('',(30.,-0.41,0.3));
#20500=CARTESIAN_POINT('',(-0.05,-1.,0.3));
#20501=CARTESIAN_POINT('Origin',(-0.1,-0.82,0.55));
#20502=CARTESIAN_POINT('',(-1.,-0.82,0.55));
#20503=CARTESIAN_POINT('',(-1.,-0.82,0.275));
#20504=CARTESIAN_POINT('',(30.,-0.82,0.55));
#20505=CARTESIAN_POINT('',(-0.1,-0.82,0.55));
#20506=CARTESIAN_POINT('',(30.,-0.82,0.275));
#20507=CARTESIAN_POINT('Origin',(-0.1,-0.67,0.55));
#20508=CARTESIAN_POINT('',(-1.,-0.67,0.55));
#20509=CARTESIAN_POINT('',(-1.,-0.335,0.55));
#20510=CARTESIAN_POINT('',(30.,-0.67,0.55));
#20511=CARTESIAN_POINT('',(-0.1,-0.67,0.55));
#20512=CARTESIAN_POINT('',(30.,-0.335,0.55));
#20513=CARTESIAN_POINT('Origin',(-0.1,-0.42,0.3));
#20514=CARTESIAN_POINT('',(-1.,-0.42,0.3));
#20515=CARTESIAN_POINT('',(-1.,-0.24,0.12));
#20516=CARTESIAN_POINT('',(30.,-0.42,0.3));
#20517=CARTESIAN_POINT('',(-0.1,-0.42,0.3));
#20518=CARTESIAN_POINT('',(30.,-0.24,0.12));
#20519=CARTESIAN_POINT('Origin',(-0.1,-0.42,-0.3));
#20520=CARTESIAN_POINT('',(-1.,-0.42,-0.3));
#20521=CARTESIAN_POINT('',(-1.,-0.42,-0.15));
#20522=CARTESIAN_POINT('',(30.,-0.42,-0.3));
#20523=CARTESIAN_POINT('',(-0.1,-0.42,-0.3));
#20524=CARTESIAN_POINT('',(30.,-0.42,-0.15));
#20525=CARTESIAN_POINT('Origin',(-0.1,-0.67,-0.55));
#20526=CARTESIAN_POINT('',(-1.,-0.67,-0.55));
#20527=CARTESIAN_POINT('',(-1.,-0.365,-0.245));
#20528=CARTESIAN_POINT('',(30.,-0.67,-0.55));
#20529=CARTESIAN_POINT('',(-0.1,-0.67,-0.55));
#20530=CARTESIAN_POINT('',(30.,-0.365,-0.245));
#20531=CARTESIAN_POINT('Origin',(-0.1,-0.82,-0.55));
#20532=CARTESIAN_POINT('',(-1.,-0.82,-0.55));
#20533=CARTESIAN_POINT('',(-1.,-0.41,-0.55));
#20534=CARTESIAN_POINT('',(30.,-0.82,-0.55));
#20535=CARTESIAN_POINT('',(-0.1,-0.82,-0.55));
#20536=CARTESIAN_POINT('',(30.,-0.41,-0.55));
#20537=CARTESIAN_POINT('Origin',(-0.1,-0.82,-0.3));
#20538=CARTESIAN_POINT('',(-1.,-0.82,-0.3));
#20539=CARTESIAN_POINT('',(-1.,-0.82,-0.15));
#20540=CARTESIAN_POINT('',(30.,-0.82,-0.3));
#20541=CARTESIAN_POINT('',(-0.1,-0.82,-0.3));
#20542=CARTESIAN_POINT('',(30.,-0.82,-0.15));
#20543=CARTESIAN_POINT('Origin',(-0.1,-1.05,-0.3));
#20544=CARTESIAN_POINT('',(-1.,-1.,-0.3));
#20545=CARTESIAN_POINT('',(-1.,-0.525,-0.3));
#20546=CARTESIAN_POINT('',(30.,-1.,-0.3));
#20547=CARTESIAN_POINT('',(-0.05,-1.,-0.3));
#20548=CARTESIAN_POINT('',(30.,-0.525,-0.3));
#20549=CARTESIAN_POINT('Origin',(-0.1,0.3,0.82));
#20550=CARTESIAN_POINT('',(-1.,0.3,0.82));
#20551=CARTESIAN_POINT('',(-1.,0.3,1.));
#20552=CARTESIAN_POINT('',(-1.,0.3,0.41));
#20553=CARTESIAN_POINT('',(30.,0.3,0.82));
#20554=CARTESIAN_POINT('',(-0.1,0.3,0.82));
#20555=CARTESIAN_POINT('',(30.,0.3,1.));
#20556=CARTESIAN_POINT('',(30.,0.3,0.41));
#20557=CARTESIAN_POINT('',(-0.05,0.3,1.));
#20558=CARTESIAN_POINT('Origin',(-0.1,0.55,0.82));
#20559=CARTESIAN_POINT('',(-1.,0.55,0.82));
#20560=CARTESIAN_POINT('',(-1.,0.275,0.82));
#20561=CARTESIAN_POINT('',(30.,0.55,0.82));
#20562=CARTESIAN_POINT('',(-0.1,0.55,0.82));
#20563=CARTESIAN_POINT('',(30.,0.275,0.82));
#20564=CARTESIAN_POINT('Origin',(-0.1,0.55,0.67));
#20565=CARTESIAN_POINT('',(-1.,0.55,0.67));
#20566=CARTESIAN_POINT('',(-1.,0.55,0.335));
#20567=CARTESIAN_POINT('',(30.,0.55,0.67));
#20568=CARTESIAN_POINT('',(-0.1,0.55,0.67));
#20569=CARTESIAN_POINT('',(30.,0.55,0.335));
#20570=CARTESIAN_POINT('Origin',(-0.1,0.3,0.42));
#20571=CARTESIAN_POINT('',(-1.,0.3,0.42));
#20572=CARTESIAN_POINT('',(-1.,0.12,0.24));
#20573=CARTESIAN_POINT('',(30.,0.3,0.42));
#20574=CARTESIAN_POINT('',(-0.1,0.3,0.42));
#20575=CARTESIAN_POINT('',(30.,0.12,0.24));
#20576=CARTESIAN_POINT('Origin',(-0.1,-0.3,0.42));
#20577=CARTESIAN_POINT('',(-1.,-0.3,0.42));
#20578=CARTESIAN_POINT('',(-1.,-0.15,0.42));
#20579=CARTESIAN_POINT('',(30.,-0.3,0.42));
#20580=CARTESIAN_POINT('',(-0.1,-0.3,0.42));
#20581=CARTESIAN_POINT('',(30.,-0.15,0.42));
#20582=CARTESIAN_POINT('Origin',(-0.1,-0.55,0.67));
#20583=CARTESIAN_POINT('',(-1.,-0.55,0.67));
#20584=CARTESIAN_POINT('',(-1.,-0.245,0.365));
#20585=CARTESIAN_POINT('',(30.,-0.55,0.67));
#20586=CARTESIAN_POINT('',(-0.1,-0.55,0.67));
#20587=CARTESIAN_POINT('',(30.,-0.245,0.365));
#20588=CARTESIAN_POINT('Origin',(-0.1,-0.55,0.82));
#20589=CARTESIAN_POINT('',(-1.,-0.55,0.82));
#20590=CARTESIAN_POINT('',(-1.,-0.55,0.41));
#20591=CARTESIAN_POINT('',(30.,-0.55,0.82));
#20592=CARTESIAN_POINT('',(-0.1,-0.55,0.82));
#20593=CARTESIAN_POINT('',(30.,-0.55,0.41));
#20594=CARTESIAN_POINT('Origin',(-0.1,-0.3,0.82));
#20595=CARTESIAN_POINT('',(-1.,-0.3,0.82));
#20596=CARTESIAN_POINT('',(-1.,-0.15,0.82));
#20597=CARTESIAN_POINT('',(30.,-0.3,0.82));
#20598=CARTESIAN_POINT('',(-0.1,-0.3,0.82));
#20599=CARTESIAN_POINT('',(30.,-0.15,0.82));
#20600=CARTESIAN_POINT('Origin',(-0.1,-0.3,1.05));
#20601=CARTESIAN_POINT('',(-1.,-0.3,1.));
#20602=CARTESIAN_POINT('',(-1.,-0.3,0.525));
#20603=CARTESIAN_POINT('',(30.,-0.3,1.));
#20604=CARTESIAN_POINT('',(-0.05,-0.3,1.));
#20605=CARTESIAN_POINT('',(30.,-0.3,0.525));
#20606=CARTESIAN_POINT('Origin',(-0.1,0.,0.));
#20607=CARTESIAN_POINT('',(-1.,-2.57175827820944E-17,0.21));
#20608=CARTESIAN_POINT('Origin',(-1.,0.,0.));
#20609=CARTESIAN_POINT('',(30.,2.57175827820944E-17,0.21));
#20610=CARTESIAN_POINT('',(-0.1,-2.57175827820944E-17,0.21));
#20611=CARTESIAN_POINT('Origin',(30.,0.,0.));
#20612=CARTESIAN_POINT('Origin',(0.,1.,-1.));
#20613=CARTESIAN_POINT('',(-1.,1.,1.));
#20614=CARTESIAN_POINT('',(-1.,1.,-0.5));
#20615=CARTESIAN_POINT('',(30.,1.,1.));
#20616=CARTESIAN_POINT('',(0.,1.,1.));
#20617=CARTESIAN_POINT('',(30.,1.,-1.));
#20618=CARTESIAN_POINT('Origin',(0.,1.,-1.));
#20619=CARTESIAN_POINT('',(30.,1.,-1.));
#20620=CARTESIAN_POINT('',(30.,1.,-1.));
#20621=CARTESIAN_POINT('',(-1.,1.,-1.));
#20622=CARTESIAN_POINT('',(0.,1.,-1.));
#20623=CARTESIAN_POINT('',(-1.,1.,-0.5));
#20624=CARTESIAN_POINT('Origin',(0.,-1.,-1.));
#20625=CARTESIAN_POINT('',(-1.,-0.5,-1.));
#20626=CARTESIAN_POINT('',(30.,-1.,-1.));
#20627=CARTESIAN_POINT('Origin',(0.,-1.,-1.));
#20628=CARTESIAN_POINT('',(30.,-1.,-1.));
#20629=CARTESIAN_POINT('',(30.,-1.,-1.));
#20630=CARTESIAN_POINT('',(-1.,-1.,-1.));
#20631=CARTESIAN_POINT('',(0.,-1.,-1.));
#20632=CARTESIAN_POINT('',(-1.,-0.5,-1.));
#20633=CARTESIAN_POINT('Origin',(0.,-1.,1.));
#20634=CARTESIAN_POINT('',(-1.,-1.,0.5));
#20635=CARTESIAN_POINT('',(30.,-1.,1.));
#20636=CARTESIAN_POINT('Origin',(0.,-1.,1.));
#20637=CARTESIAN_POINT('',(30.,-1.,1.));
#20638=CARTESIAN_POINT('',(30.,-1.,1.));
#20639=CARTESIAN_POINT('',(-1.,-1.,1.));
#20640=CARTESIAN_POINT('',(0.,-1.,1.));
#20641=CARTESIAN_POINT('',(-1.,-1.,0.5));
#20642=CARTESIAN_POINT('Origin',(0.,1.,1.));
#20643=CARTESIAN_POINT('',(-1.,0.5,1.));
#20644=CARTESIAN_POINT('',(30.,1.,1.));
#20645=CARTESIAN_POINT('Origin',(0.,1.,1.));
#20646=CARTESIAN_POINT('',(30.,1.,1.));
#20647=CARTESIAN_POINT('',(-1.,0.5,1.));
#20648=CARTESIAN_POINT('Origin',(30.,0.,0.));
#20649=CARTESIAN_POINT('Origin',(-1.,0.,0.));
#20650=CARTESIAN_POINT('',(0.,0.,0.));
#20651=CARTESIAN_POINT('Origin',(-0.25,-0.225,0.075));
#20652=CARTESIAN_POINT('',(0.5,-0.15,0.));
#20653=CARTESIAN_POINT('',(0.5,-0.3,0.15));
#20654=CARTESIAN_POINT('',(0.5,-0.225,0.075));
#20655=CARTESIAN_POINT('',(-0.5,-0.3,0.15));
#20656=CARTESIAN_POINT('',(-0.25,-0.3,0.15));
#20657=CARTESIAN_POINT('',(-0.5,-0.15,0.));
#20658=CARTESIAN_POINT('',(-0.5,-0.075,-0.075));
#20659=CARTESIAN_POINT('',(-0.149388386429468,-0.15,0.));
#20660=CARTESIAN_POINT('',(-0.25,-0.15,0.));
#20661=CARTESIAN_POINT('',(0.149388386429468,-0.15,0.));
#20662=CARTESIAN_POINT('Origin',(0.,0.,-0.15));
#20663=CARTESIAN_POINT('',(-0.25,-0.15,0.));
#20664=CARTESIAN_POINT('Origin',(0.,0.,-0.1));
#20665=CARTESIAN_POINT('',(-0.2117,-2.59257727379495E-17,0.));
#20666=CARTESIAN_POINT('Origin',(0.,0.,0.));
#20667=CARTESIAN_POINT('',(-0.2117,2.59257727379495E-17,0.4));
#20668=CARTESIAN_POINT('',(-0.2117,-2.59257727379495E-17,-0.1));
#20669=CARTESIAN_POINT('Origin',(0.,0.,0.4));
#20670=CARTESIAN_POINT('',(-0.149388386429468,0.15,0.));
#20671=CARTESIAN_POINT('Origin',(0.,0.,0.));
#20672=CARTESIAN_POINT('',(0.149388386429468,0.15,0.));
#20673=CARTESIAN_POINT('Origin',(0.,0.,-0.15));
#20674=CARTESIAN_POINT('Origin',(0.,0.,0.));
#20675=CARTESIAN_POINT('Origin',(0.,0.,0.));
#20676=CARTESIAN_POINT('',(-0.5,0.15,0.));
#20677=CARTESIAN_POINT('',(-0.5,0.3,0.));
#20678=CARTESIAN_POINT('',(0.25,0.15,0.));
#20679=CARTESIAN_POINT('Origin',(0.,0.,0.));
#20680=CARTESIAN_POINT('',(0.5,0.15,0.));
#20681=CARTESIAN_POINT('',(0.25,0.15,0.));
#20682=CARTESIAN_POINT('',(0.5,-0.3,0.));
#20683=CARTESIAN_POINT('Origin',(0.25,0.225,0.075));
#20684=CARTESIAN_POINT('',(-0.5,0.3,0.15));
#20685=CARTESIAN_POINT('',(-0.5,0.225,0.075));
#20686=CARTESIAN_POINT('',(0.5,0.3,0.15));
#20687=CARTESIAN_POINT('',(0.25,0.3,0.15));
#20688=CARTESIAN_POINT('',(0.5,0.075,-0.075));
#20689=CARTESIAN_POINT('Origin',(0.5,-0.3,0.));
#20690=CARTESIAN_POINT('',(0.5,0.3,0.4));
#20691=CARTESIAN_POINT('',(0.5,0.3,0.));
#20692=CARTESIAN_POINT('',(0.5,-0.3,0.4));
#20693=CARTESIAN_POINT('',(0.5,-0.3,0.4));
#20694=CARTESIAN_POINT('',(0.5,-0.3,0.));
#20695=CARTESIAN_POINT('Origin',(0.5,0.3,0.));
#20696=CARTESIAN_POINT('',(-0.5,0.3,0.4));
#20697=CARTESIAN_POINT('',(-0.5,0.3,0.));
#20698=CARTESIAN_POINT('',(0.5,0.3,0.4));
#20699=CARTESIAN_POINT('Origin',(-0.5,-0.3,0.));
#20700=CARTESIAN_POINT('',(-0.5,-0.3,0.4));
#20701=CARTESIAN_POINT('',(-0.5,-0.3,0.4));
#20702=CARTESIAN_POINT('',(-0.5,-0.3,0.));
#20703=CARTESIAN_POINT('Origin',(-0.5,0.3,0.));
#20704=CARTESIAN_POINT('',(-0.5,0.3,0.4));
#20705=CARTESIAN_POINT('Origin',(0.,0.,0.4));
#20706=CARTESIAN_POINT('',(0.,0.,0.));
#20707=CARTESIAN_POINT('Origin',(0.,0.09,0.));
#20708=CARTESIAN_POINT('',(-0.285,0.1,3.49024337756996E-17));
#20709=CARTESIAN_POINT('Origin',(0.,0.1,0.));
#20710=CARTESIAN_POINT('',(-0.265,0.08,-3.24531401774049E-17));
#20711=CARTESIAN_POINT('',(-0.275,0.09,3.36777869765522E-17));
#20712=CARTESIAN_POINT('Origin',(0.,0.08,0.));
#20713=CARTESIAN_POINT('Origin',(0.,0.,0.));
#20714=CARTESIAN_POINT('',(-0.265,0.,3.24531401774049E-17));
#20715=CARTESIAN_POINT('',(-0.265,0.,3.24531401774049E-17));
#20716=CARTESIAN_POINT('Origin',(0.,0.,0.));
#20717=CARTESIAN_POINT('Origin',(0.,0.1,0.));
#20718=CARTESIAN_POINT('',(-0.5,0.1,6.12323399573677E-17));
#20719=CARTESIAN_POINT('Origin',(0.,0.1,0.));
#20720=CARTESIAN_POINT('Origin',(0.,0.,0.));
#20721=CARTESIAN_POINT('',(-0.5,0.,6.12323399573677E-17));
#20722=CARTESIAN_POINT('',(-0.5,0.,6.12323399573677E-17));
#20723=CARTESIAN_POINT('Origin',(0.,0.,0.));
#20724=CARTESIAN_POINT('Origin',(0.,0.,0.));
#20725=CARTESIAN_POINT('',(0.,0.,0.));
#20726=CARTESIAN_POINT('Origin',(0.115470053837925,-0.5,-0.2));
#20727=CARTESIAN_POINT('',(0.23094010767585,-0.5,0.));
#20728=CARTESIAN_POINT('',(0.115470053837925,-0.5,-0.2));
#20729=CARTESIAN_POINT('',(0.23094010767585,-0.5,0.));
#20730=CARTESIAN_POINT('',(0.115470053837925,-0.8,-0.2));
#20731=CARTESIAN_POINT('',(0.115470053837925,-0.5,-0.2));
#20732=CARTESIAN_POINT('',(0.23094010767585,-0.8,0.));
#20733=CARTESIAN_POINT('',(0.23094010767585,-0.8,0.));
#20734=CARTESIAN_POINT('',(0.23094010767585,-0.5,0.));
#20735=CARTESIAN_POINT('Origin',(-0.115470053837925,-0.5,-0.2));
#20736=CARTESIAN_POINT('',(-0.115470053837925,-0.5,-0.2));
#20737=CARTESIAN_POINT('',(0.115470053837925,-0.5,-0.2));
#20738=CARTESIAN_POINT('',(-0.115470053837925,-0.8,-0.2));
#20739=CARTESIAN_POINT('',(-0.115470053837925,-0.5,-0.2));
#20740=CARTESIAN_POINT('',(0.115470053837925,-0.8,-0.2));
#20741=CARTESIAN_POINT('Origin',(-0.23094010767585,-0.5,-2.77555756156289E-17));
#20742=CARTESIAN_POINT('',(-0.23094010767585,-0.5,-2.82820063659975E-17));
#20743=CARTESIAN_POINT('',(-0.115470053837925,-0.5,-0.2));
#20744=CARTESIAN_POINT('',(-0.23094010767585,-0.8,-2.77555756156289E-17));
#20745=CARTESIAN_POINT('',(-0.23094010767585,-0.5,-2.82820063659975E-17));
#20746=CARTESIAN_POINT('',(-0.115470053837925,-0.8,-0.2));
#20747=CARTESIAN_POINT('Origin',(-0.115470053837925,-0.5,0.2));
#20748=CARTESIAN_POINT('',(-0.115470053837925,-0.5,0.2));
#20749=CARTESIAN_POINT('',(-0.23094010767585,-0.5,-2.82820063659975E-17));
#20750=CARTESIAN_POINT('',(-0.115470053837925,-0.8,0.2));
#20751=CARTESIAN_POINT('',(-0.115470053837925,-0.5,0.2));
#20752=CARTESIAN_POINT('',(-0.23094010767585,-0.8,-2.82820063659975E-17));
#20753=CARTESIAN_POINT('Origin',(0.115470053837925,-0.5,0.2));
#20754=CARTESIAN_POINT('',(0.115470053837925,-0.5,0.2));
#20755=CARTESIAN_POINT('',(-0.115470053837925,-0.5,0.2));
#20756=CARTESIAN_POINT('',(0.115470053837925,-0.8,0.2));
#20757=CARTESIAN_POINT('',(0.115470053837925,-0.5,0.2));
#20758=CARTESIAN_POINT('',(-0.115470053837925,-0.8,0.2));
#20759=CARTESIAN_POINT('Origin',(0.23094010767585,-0.5,0.));
#20760=CARTESIAN_POINT('',(0.115470053837925,-0.5,0.2));
#20761=CARTESIAN_POINT('',(0.115470053837925,-0.8,0.2));
#20762=CARTESIAN_POINT('Origin',(0.,-0.5,0.));
#20763=CARTESIAN_POINT('Origin',(0.,-0.8,0.));
#20764=CARTESIAN_POINT('Origin',(0.,-1.8,0.));
#20765=CARTESIAN_POINT('',(-0.24505,-1.8,3.00099698131059E-17));
#20766=CARTESIAN_POINT('Origin',(0.,-1.8,0.));
#20767=CARTESIAN_POINT('Origin',(0.375,0.5,0.));
#20768=CARTESIAN_POINT('',(-0.375,0.5,-4.59242549680257E-17));
#20769=CARTESIAN_POINT('Origin',(0.,0.5,0.));
#20770=CARTESIAN_POINT('Origin',(0.,0.475,0.));
#20771=CARTESIAN_POINT('',(-0.425,0.45,-5.20474889637625E-17));
#20772=CARTESIAN_POINT('Origin',(0.,0.45,0.));
#20773=CARTESIAN_POINT('',(-0.4,0.475,-4.89858719658941E-17));
#20774=CARTESIAN_POINT('Origin',(0.,0.24,0.));
#20775=CARTESIAN_POINT('',(-0.425,0.0299999999999998,-5.20474889637625E-17));
#20776=CARTESIAN_POINT('Origin',(0.,0.0299999999999998,0.));
#20777=CARTESIAN_POINT('',(-0.425,0.24,-5.20474889637625E-17));
#20778=CARTESIAN_POINT('Origin',(0.,0.0150000000000001,0.));
#20779=CARTESIAN_POINT('',(-0.395,4.85722573273506E-17,-4.83735485663204E-17));
#20780=CARTESIAN_POINT('Origin',(0.,0.,0.));
#20781=CARTESIAN_POINT('',(-0.41,0.0150000000000001,-5.02105187650415E-17));
#20782=CARTESIAN_POINT('Origin',(0.27,0.,0.));
#20783=CARTESIAN_POINT('',(-0.27,0.,-3.30654635769785E-17));
#20784=CARTESIAN_POINT('Origin',(0.,0.,0.));
#20785=CARTESIAN_POINT('Origin',(0.,-0.02,0.));
#20786=CARTESIAN_POINT('',(-0.24505,-0.0498999999999999,3.00099698131059E-17));
#20787=CARTESIAN_POINT('Origin',(0.,-0.0498999999999999,0.));
#20788=CARTESIAN_POINT('',(-0.26,-0.02,-3.18408167778312E-17));
#20789=CARTESIAN_POINT('Origin',(0.,-0.995,0.));
#20790=CARTESIAN_POINT('',(-0.24505,-0.995,-3.00099698131059E-17));
#20791=CARTESIAN_POINT('',(0.,0.,0.));
#20792=CARTESIAN_POINT('',(0.,0.,0.));
#20793=CARTESIAN_POINT('Origin',(15.,-7.9,5.1));
#20794=CARTESIAN_POINT('',(14.725,-7.9,5.2));
#20795=CARTESIAN_POINT('Origin',(15.,-7.9,5.2));
#20796=CARTESIAN_POINT('',(14.725,-7.9,6.));
#20797=CARTESIAN_POINT('',(14.725,-7.9,5.1));
#20798=CARTESIAN_POINT('Origin',(15.,-7.9,6.));
#20799=CARTESIAN_POINT('Origin',(12.,-4.1,5.1));
#20800=CARTESIAN_POINT('',(11.725,-4.1,5.2));
#20801=CARTESIAN_POINT('Origin',(12.,-4.1,5.2));
#20802=CARTESIAN_POINT('',(11.725,-4.1,6.));
#20803=CARTESIAN_POINT('',(11.725,-4.1,5.1));
#20804=CARTESIAN_POINT('Origin',(12.,-4.1,6.));
#20805=CARTESIAN_POINT('Origin',(12.,-7.9,5.1));
#20806=CARTESIAN_POINT('',(11.725,-7.9,5.2));
#20807=CARTESIAN_POINT('Origin',(12.,-7.9,5.2));
#20808=CARTESIAN_POINT('',(11.725,-7.9,6.));
#20809=CARTESIAN_POINT('',(11.725,-7.9,5.1));
#20810=CARTESIAN_POINT('Origin',(12.,-7.9,6.));
#20811=CARTESIAN_POINT('Origin',(15.,-4.1,5.1));
#20812=CARTESIAN_POINT('',(14.725,-4.1,5.2));
#20813=CARTESIAN_POINT('Origin',(15.,-4.1,5.2));
#20814=CARTESIAN_POINT('',(14.725,-4.1,6.));
#20815=CARTESIAN_POINT('',(14.725,-4.1,5.1));
#20816=CARTESIAN_POINT('Origin',(15.,-4.1,6.));
#20817=CARTESIAN_POINT('Origin',(16.6,-3.65,5.2));
#20818=CARTESIAN_POINT('',(16.6,-3.65,5.2));
#20819=CARTESIAN_POINT('',(10.4,-3.65,5.2));
#20820=CARTESIAN_POINT('',(16.6,-3.65,5.2));
#20821=CARTESIAN_POINT('',(10.4,-3.65,6.));
#20822=CARTESIAN_POINT('',(10.4,-3.65,5.2));
#20823=CARTESIAN_POINT('',(16.6,-3.65,6.));
#20824=CARTESIAN_POINT('',(16.6,-3.65,6.));
#20825=CARTESIAN_POINT('',(16.6,-3.65,5.2));
#20826=CARTESIAN_POINT('Origin',(16.6,-8.35,5.2));
#20827=CARTESIAN_POINT('',(16.6,-8.35,5.2));
#20828=CARTESIAN_POINT('',(16.6,-8.35,5.2));
#20829=CARTESIAN_POINT('',(16.6,-8.35,6.));
#20830=CARTESIAN_POINT('',(16.6,-8.35,6.));
#20831=CARTESIAN_POINT('',(16.6,-8.35,5.2));
#20832=CARTESIAN_POINT('Origin',(10.4,-8.35,5.2));
#20833=CARTESIAN_POINT('',(10.4,-8.35,5.2));
#20834=CARTESIAN_POINT('',(10.4,-8.35,5.2));
#20835=CARTESIAN_POINT('',(10.4,-8.35,6.));
#20836=CARTESIAN_POINT('',(10.4,-8.35,6.));
#20837=CARTESIAN_POINT('',(10.4,-8.35,5.2));
#20838=CARTESIAN_POINT('Origin',(10.4,-3.65,5.2));
#20839=CARTESIAN_POINT('',(10.4,-3.65,5.2));
#20840=CARTESIAN_POINT('',(10.4,-3.65,6.));
#20841=CARTESIAN_POINT('Origin',(13.5,-6.,6.));
#20842=CARTESIAN_POINT('Origin',(13.5,-6.,5.2));
#20843=CARTESIAN_POINT('',(0.,0.,0.));
#20844=CARTESIAN_POINT('Origin',(14.,-1.5,5.9));
#20845=CARTESIAN_POINT('',(13.725,-1.5,6.));
#20846=CARTESIAN_POINT('Origin',(14.,-1.5,6.));
#20847=CARTESIAN_POINT('',(13.725,-1.5,7.2));
#20848=CARTESIAN_POINT('',(13.725,-1.5,5.9));
#20849=CARTESIAN_POINT('Origin',(14.,-1.5,7.2));
#20850=CARTESIAN_POINT('Origin',(12.5,1.5,5.9));
#20851=CARTESIAN_POINT('',(12.225,1.5,6.));
#20852=CARTESIAN_POINT('Origin',(12.5,1.5,6.));
#20853=CARTESIAN_POINT('',(12.225,1.5,7.2));
#20854=CARTESIAN_POINT('',(12.225,1.5,5.9));
#20855=CARTESIAN_POINT('Origin',(12.5,1.5,7.2));
#20856=CARTESIAN_POINT('Origin',(12.5,-1.5,5.9));
#20857=CARTESIAN_POINT('',(12.225,-1.5,6.));
#20858=CARTESIAN_POINT('Origin',(12.5,-1.5,6.));
#20859=CARTESIAN_POINT('',(12.225,-1.5,7.2));
#20860=CARTESIAN_POINT('',(12.225,-1.5,5.9));
#20861=CARTESIAN_POINT('Origin',(12.5,-1.5,7.2));
#20862=CARTESIAN_POINT('Origin',(14.,1.5,5.9));
#20863=CARTESIAN_POINT('',(13.725,1.5,6.));
#20864=CARTESIAN_POINT('Origin',(14.,1.5,6.));
#20865=CARTESIAN_POINT('',(13.725,1.5,7.2));
#20866=CARTESIAN_POINT('',(13.725,1.5,5.9));
#20867=CARTESIAN_POINT('Origin',(14.,1.5,7.2));
#20868=CARTESIAN_POINT('Origin',(15.,-7.9,5.1));
#20869=CARTESIAN_POINT('',(14.725,-7.9,6.));
#20870=CARTESIAN_POINT('Origin',(15.,-7.9,6.));
#20871=CARTESIAN_POINT('',(14.725,-7.9,7.2));
#20872=CARTESIAN_POINT('',(14.725,-7.9,5.1));
#20873=CARTESIAN_POINT('Origin',(15.,-7.9,7.2));
#20874=CARTESIAN_POINT('Origin',(12.,-4.1,5.1));
#20875=CARTESIAN_POINT('',(11.725,-4.1,6.));
#20876=CARTESIAN_POINT('Origin',(12.,-4.1,6.));
#20877=CARTESIAN_POINT('',(11.725,-4.1,7.2));
#20878=CARTESIAN_POINT('',(11.725,-4.1,5.1));
#20879=CARTESIAN_POINT('Origin',(12.,-4.1,7.2));
#20880=CARTESIAN_POINT('Origin',(12.,-7.9,5.1));
#20881=CARTESIAN_POINT('',(11.725,-7.9,6.));
#20882=CARTESIAN_POINT('Origin',(12.,-7.9,6.));
#20883=CARTESIAN_POINT('',(11.725,-7.9,7.2));
#20884=CARTESIAN_POINT('',(11.725,-7.9,5.1));
#20885=CARTESIAN_POINT('Origin',(12.,-7.9,7.2));
#20886=CARTESIAN_POINT('Origin',(15.,-4.1,5.1));
#20887=CARTESIAN_POINT('',(14.725,-4.1,6.));
#20888=CARTESIAN_POINT('Origin',(15.,-4.1,6.));
#20889=CARTESIAN_POINT('',(14.725,-4.1,7.2));
#20890=CARTESIAN_POINT('',(14.725,-4.1,5.1));
#20891=CARTESIAN_POINT('Origin',(15.,-4.1,7.2));
#20892=CARTESIAN_POINT('Origin',(17.,2.5,6.));
#20893=CARTESIAN_POINT('',(17.,2.5,6.));
#20894=CARTESIAN_POINT('',(10.,2.5,6.));
#20895=CARTESIAN_POINT('',(17.,2.5,6.));
#20896=CARTESIAN_POINT('',(10.,2.5,7.2));
#20897=CARTESIAN_POINT('',(10.,2.5,6.));
#20898=CARTESIAN_POINT('',(17.,2.5,7.2));
#20899=CARTESIAN_POINT('',(17.,2.5,7.2));
#20900=CARTESIAN_POINT('',(17.,2.5,6.));
#20901=CARTESIAN_POINT('Origin',(17.,-10.,6.));
#20902=CARTESIAN_POINT('',(17.,-10.,6.));
#20903=CARTESIAN_POINT('',(17.,-10.,6.));
#20904=CARTESIAN_POINT('',(17.,-10.,7.2));
#20905=CARTESIAN_POINT('',(17.,-10.,7.2));
#20906=CARTESIAN_POINT('',(17.,-10.,6.));
#20907=CARTESIAN_POINT('Origin',(10.,-10.,6.));
#20908=CARTESIAN_POINT('',(10.,-10.,6.));
#20909=CARTESIAN_POINT('',(10.,-10.,6.));
#20910=CARTESIAN_POINT('',(10.,-10.,7.2));
#20911=CARTESIAN_POINT('',(10.,-10.,7.2));
#20912=CARTESIAN_POINT('',(10.,-10.,6.));
#20913=CARTESIAN_POINT('Origin',(10.,2.5,6.));
#20914=CARTESIAN_POINT('',(10.,2.5,6.));
#20915=CARTESIAN_POINT('',(10.,2.5,7.2));
#20916=CARTESIAN_POINT('Origin',(13.5,-3.75,7.2));
#20917=CARTESIAN_POINT('Origin',(13.5,-3.75,6.));
#20918=CARTESIAN_POINT('',(0.,0.,0.));
#20919=CARTESIAN_POINT('Origin',(14.,-1.5,5.1));
#20920=CARTESIAN_POINT('',(13.79,-1.5,5.1));
#20921=CARTESIAN_POINT('Origin',(14.,-1.5,5.1));
#20922=CARTESIAN_POINT('',(13.79,-1.5,6.));
#20923=CARTESIAN_POINT('',(13.79,-1.5,5.1));
#20924=CARTESIAN_POINT('Origin',(14.,-1.5,6.));
#20925=CARTESIAN_POINT('Origin',(14.,-1.5,5.1));
#20926=CARTESIAN_POINT('Origin',(12.5,1.5,5.1));
#20927=CARTESIAN_POINT('',(12.29,1.5,5.1));
#20928=CARTESIAN_POINT('Origin',(12.5,1.5,5.1));
#20929=CARTESIAN_POINT('',(12.29,1.5,6.));
#20930=CARTESIAN_POINT('',(12.29,1.5,5.1));
#20931=CARTESIAN_POINT('Origin',(12.5,1.5,6.));
#20932=CARTESIAN_POINT('Origin',(12.5,1.5,5.1));
#20933=CARTESIAN_POINT('Origin',(12.5,-1.5,5.1));
#20934=CARTESIAN_POINT('',(12.29,-1.5,5.1));
#20935=CARTESIAN_POINT('Origin',(12.5,-1.5,5.1));
#20936=CARTESIAN_POINT('',(12.29,-1.5,6.));
#20937=CARTESIAN_POINT('',(12.29,-1.5,5.1));
#20938=CARTESIAN_POINT('Origin',(12.5,-1.5,6.));
#20939=CARTESIAN_POINT('Origin',(12.5,-1.5,5.1));
#20940=CARTESIAN_POINT('Origin',(14.,1.5,5.1));
#20941=CARTESIAN_POINT('',(13.79,1.5,5.1));
#20942=CARTESIAN_POINT('Origin',(14.,1.5,5.1));
#20943=CARTESIAN_POINT('',(13.79,1.5,6.));
#20944=CARTESIAN_POINT('',(13.79,1.5,5.1));
#20945=CARTESIAN_POINT('Origin',(14.,1.5,6.));
#20946=CARTESIAN_POINT('Origin',(14.,1.5,5.1));
#20947=CARTESIAN_POINT('Origin',(12.9,-1.5,4.));
#20948=CARTESIAN_POINT('',(12.9,-1.5,4.165));
#20949=CARTESIAN_POINT('Origin',(12.9,-1.5,4.));
#20950=CARTESIAN_POINT('',(14.5,-1.5,4.165));
#20951=CARTESIAN_POINT('',(12.9,-1.5,4.165));
#20952=CARTESIAN_POINT('Origin',(14.5,-1.5,4.));
#20953=CARTESIAN_POINT('Origin',(12.9,-1.5,4.));
#20954=CARTESIAN_POINT('Origin',(12.9,1.5,4.));
#20955=CARTESIAN_POINT('',(12.9,1.5,4.165));
#20956=CARTESIAN_POINT('Origin',(12.9,1.5,4.));
#20957=CARTESIAN_POINT('',(14.5,1.5,4.165));
#20958=CARTESIAN_POINT('',(12.9,1.5,4.165));
#20959=CARTESIAN_POINT('Origin',(14.5,1.5,4.));
#20960=CARTESIAN_POINT('Origin',(12.9,1.5,4.));
#20961=CARTESIAN_POINT('Origin',(12.9,0.,5.5));
#20962=CARTESIAN_POINT('',(12.9,-2.02066721859313E-17,5.665));
#20963=CARTESIAN_POINT('Origin',(12.9,0.,5.5));
#20964=CARTESIAN_POINT('',(14.5,2.02066721859313E-17,5.665));
#20965=CARTESIAN_POINT('',(12.9,-2.02066721859313E-17,5.665));
#20966=CARTESIAN_POINT('Origin',(14.5,0.,5.5));
#20967=CARTESIAN_POINT('Origin',(12.9,0.,5.5));
#20968=CARTESIAN_POINT('Origin',(11.9,0.,4.));
#20969=CARTESIAN_POINT('',(12.,-1.35935794705356E-16,5.11));
#20970=CARTESIAN_POINT('Origin',(12.,0.,4.));
#20971=CARTESIAN_POINT('',(14.5,1.35935794705356E-16,5.11));
#20972=CARTESIAN_POINT('',(11.9,-1.35935794705356E-16,5.11));
#20973=CARTESIAN_POINT('Origin',(14.5,0.,4.));
#20974=CARTESIAN_POINT('Origin',(14.5,2.2,2.5));
#20975=CARTESIAN_POINT('',(14.5,2.2,2.5));
#20976=CARTESIAN_POINT('',(12.,2.2,2.5));
#20977=CARTESIAN_POINT('',(14.5,2.2,2.5));
#20978=CARTESIAN_POINT('',(12.,2.2,6.));
#20979=CARTESIAN_POINT('',(12.,2.2,2.5));
#20980=CARTESIAN_POINT('',(14.5,2.2,6.));
#20981=CARTESIAN_POINT('',(14.5,2.2,6.));
#20982=CARTESIAN_POINT('',(14.5,2.2,2.5));
#20983=CARTESIAN_POINT('Origin',(14.5,-2.2,2.5));
#20984=CARTESIAN_POINT('',(14.5,-2.2,2.5));
#20985=CARTESIAN_POINT('',(14.5,-2.2,2.5));
#20986=CARTESIAN_POINT('',(14.5,-2.2,6.));
#20987=CARTESIAN_POINT('',(14.5,-2.2,6.));
#20988=CARTESIAN_POINT('',(14.5,-2.2,2.5));
#20989=CARTESIAN_POINT('Origin',(12.,-2.2,2.5));
#20990=CARTESIAN_POINT('',(12.,-2.2,2.5));
#20991=CARTESIAN_POINT('',(12.,-2.2,2.5));
#20992=CARTESIAN_POINT('',(12.,-2.2,6.));
#20993=CARTESIAN_POINT('',(12.,-2.2,6.));
#20994=CARTESIAN_POINT('',(12.,-2.2,2.5));
#20995=CARTESIAN_POINT('Origin',(12.,2.2,2.5));
#20996=CARTESIAN_POINT('',(12.,2.2,2.5));
#20997=CARTESIAN_POINT('',(12.,2.2,6.));
#20998=CARTESIAN_POINT('Origin',(13.25,0.,6.));
#20999=CARTESIAN_POINT('Origin',(13.25,0.,2.5));
#21000=CARTESIAN_POINT('',(0.,0.,0.));
#21001=CARTESIAN_POINT('',(0.,0.,0.));
#21002=CARTESIAN_POINT('Origin',(1.5,-1.9,1.7));
#21003=CARTESIAN_POINT('',(1.56403124237433,-1.7,1.7));
#21004=CARTESIAN_POINT('',(1.43596875762567,-1.7,1.7));
#21005=CARTESIAN_POINT('',(0.75,-1.7,1.7));
#21006=CARTESIAN_POINT('Origin',(1.5,-1.9,1.7));
#21007=CARTESIAN_POINT('Origin',(1.5,-1.9,1.7));
#21008=CARTESIAN_POINT('',(1.56403124237433,-1.7,1.75));
#21009=CARTESIAN_POINT('',(1.56403124237433,-1.7,1.7));
#21010=CARTESIAN_POINT('',(1.29,-1.9,1.75));
#21011=CARTESIAN_POINT('Origin',(1.5,-1.9,1.75));
#21012=CARTESIAN_POINT('',(1.29,-1.9,2.4));
#21013=CARTESIAN_POINT('',(1.29,-1.9,1.7));
#21014=CARTESIAN_POINT('Origin',(1.5,-1.9,2.4));
#21015=CARTESIAN_POINT('',(1.43596875762567,-1.7,1.75));
#21016=CARTESIAN_POINT('Origin',(1.5,-1.9,1.75));
#21017=CARTESIAN_POINT('',(1.43596875762567,-1.7,1.7));
#21018=CARTESIAN_POINT('Origin',(-1.5,1.9,1.7));
#21019=CARTESIAN_POINT('',(-1.56403124237433,1.7,1.7));
#21020=CARTESIAN_POINT('',(-1.43596875762567,1.7,1.7));
#21021=CARTESIAN_POINT('',(-0.75,1.7,1.7));
#21022=CARTESIAN_POINT('Origin',(-1.5,1.9,1.7));
#21023=CARTESIAN_POINT('Origin',(-1.5,1.9,1.7));
#21024=CARTESIAN_POINT('',(-1.56403124237433,1.7,1.75));
#21025=CARTESIAN_POINT('',(-1.56403124237433,1.7,1.7));
#21026=CARTESIAN_POINT('',(-1.71,1.9,1.75));
#21027=CARTESIAN_POINT('Origin',(-1.5,1.9,1.75));
#21028=CARTESIAN_POINT('',(-1.71,1.9,2.4));
#21029=CARTESIAN_POINT('',(-1.71,1.9,1.7));
#21030=CARTESIAN_POINT('Origin',(-1.5,1.9,2.4));
#21031=CARTESIAN_POINT('',(-1.43596875762567,1.7,1.75));
#21032=CARTESIAN_POINT('Origin',(-1.5,1.9,1.75));
#21033=CARTESIAN_POINT('',(-1.43596875762567,1.7,1.7));
#21034=CARTESIAN_POINT('Origin',(-1.5,-1.9,1.7));
#21035=CARTESIAN_POINT('',(-1.43596875762567,-1.7,1.7));
#21036=CARTESIAN_POINT('',(-1.56403124237433,-1.7,1.7));
#21037=CARTESIAN_POINT('',(-0.75,-1.7,1.7));
#21038=CARTESIAN_POINT('Origin',(-1.5,-1.9,1.7));
#21039=CARTESIAN_POINT('Origin',(-1.5,-1.9,1.7));
#21040=CARTESIAN_POINT('',(-1.43596875762567,-1.7,1.75));
#21041=CARTESIAN_POINT('',(-1.43596875762567,-1.7,1.7));
#21042=CARTESIAN_POINT('',(-1.71,-1.9,1.75));
#21043=CARTESIAN_POINT('Origin',(-1.5,-1.9,1.75));
#21044=CARTESIAN_POINT('',(-1.71,-1.9,2.4));
#21045=CARTESIAN_POINT('',(-1.71,-1.9,1.7));
#21046=CARTESIAN_POINT('Origin',(-1.5,-1.9,2.4));
#21047=CARTESIAN_POINT('',(-1.56403124237433,-1.7,1.75));
#21048=CARTESIAN_POINT('Origin',(-1.5,-1.9,1.75));
#21049=CARTESIAN_POINT('',(-1.56403124237433,-1.7,1.7));
#21050=CARTESIAN_POINT('Origin',(1.5,1.9,1.7));
#21051=CARTESIAN_POINT('',(1.43596875762567,1.7,1.7));
#21052=CARTESIAN_POINT('',(1.56403124237433,1.7,1.7));
#21053=CARTESIAN_POINT('',(0.75,1.7,1.7));
#21054=CARTESIAN_POINT('Origin',(1.5,1.9,1.7));
#21055=CARTESIAN_POINT('Origin',(1.5,1.9,1.7));
#21056=CARTESIAN_POINT('',(1.43596875762567,1.7,1.75));
#21057=CARTESIAN_POINT('',(1.43596875762567,1.7,1.7));
#21058=CARTESIAN_POINT('',(1.29,1.9,1.75));
#21059=CARTESIAN_POINT('Origin',(1.5,1.9,1.75));
#21060=CARTESIAN_POINT('',(1.29,1.9,2.4));
#21061=CARTESIAN_POINT('',(1.29,1.9,1.7));
#21062=CARTESIAN_POINT('Origin',(1.5,1.9,2.4));
#21063=CARTESIAN_POINT('',(1.56403124237433,1.7,1.75));
#21064=CARTESIAN_POINT('Origin',(1.5,1.9,1.75));
#21065=CARTESIAN_POINT('',(1.56403124237433,1.7,1.7));
#21066=CARTESIAN_POINT('Origin',(0.,-1.7,1.75));
#21067=CARTESIAN_POINT('',(0.,-1.7,1.75));
#21068=CARTESIAN_POINT('',(-1.97,-1.7,1.75));
#21069=CARTESIAN_POINT('',(0.,-1.7,1.75));
#21070=CARTESIAN_POINT('',(-1.97,-1.7,0.43));
#21071=CARTESIAN_POINT('',(-1.97,-1.7,1.75));
#21072=CARTESIAN_POINT('',(1.97,-1.7,0.43));
#21073=CARTESIAN_POINT('',(0.,-1.7,0.43));
#21074=CARTESIAN_POINT('',(1.97,-1.7,1.75));
#21075=CARTESIAN_POINT('',(1.97,-1.7,1.75));
#21076=CARTESIAN_POINT('',(0.,-1.7,1.75));
#21077=CARTESIAN_POINT('Origin',(0.,1.7,0.43));
#21078=CARTESIAN_POINT('',(0.,1.7,1.75));
#21079=CARTESIAN_POINT('',(1.97,1.7,1.75));
#21080=CARTESIAN_POINT('',(0.,1.7,1.75));
#21081=CARTESIAN_POINT('',(1.97,1.7,0.43));
#21082=CARTESIAN_POINT('',(1.97,1.7,0.43));
#21083=CARTESIAN_POINT('',(-1.97,1.7,0.43));
#21084=CARTESIAN_POINT('',(0.,1.7,0.43));
#21085=CARTESIAN_POINT('',(-1.97,1.7,1.75));
#21086=CARTESIAN_POINT('',(-1.97,1.7,0.43));
#21087=CARTESIAN_POINT('',(0.,1.7,1.75));
#21088=CARTESIAN_POINT('Origin',(-1.97,0.,1.415));
#21089=CARTESIAN_POINT('',(-1.97,-2.35,1.75));
#21090=CARTESIAN_POINT('',(-1.97,-2.35,1.75));
#21091=CARTESIAN_POINT('',(-1.97,-2.35,2.4));
#21092=CARTESIAN_POINT('',(-1.97,-2.35,2.4));
#21093=CARTESIAN_POINT('',(-1.97,2.35,2.4));
#21094=CARTESIAN_POINT('',(-1.97,2.35,2.4));
#21095=CARTESIAN_POINT('',(-1.97,2.35,1.75));
#21096=CARTESIAN_POINT('',(-1.97,2.35,1.75));
#21097=CARTESIAN_POINT('',(-1.97,1.7,1.75));
#21098=CARTESIAN_POINT('',(-1.97,0.78,0.43));
#21099=CARTESIAN_POINT('',(-1.97,0.78,0.43));
#21100=CARTESIAN_POINT('',(-1.97,0.78,1.55));
#21101=CARTESIAN_POINT('',(-1.97,0.78,1.55));
#21102=CARTESIAN_POINT('',(-1.97,-0.78,1.55));
#21103=CARTESIAN_POINT('',(-1.97,-0.78,1.55));
#21104=CARTESIAN_POINT('',(-1.97,-0.78,0.43));
#21105=CARTESIAN_POINT('',(-1.97,-0.78,0.43));
#21106=CARTESIAN_POINT('',(-1.97,-1.7,0.43));
#21107=CARTESIAN_POINT('Origin',(0.,-2.35,1.75));
#21108=CARTESIAN_POINT('',(1.97,-2.35,1.75));
#21109=CARTESIAN_POINT('',(1.97,-2.35,1.75));
#21110=CARTESIAN_POINT('',(0.,-2.35,1.75));
#21111=CARTESIAN_POINT('Origin',(0.,-2.35,2.4));
#21112=CARTESIAN_POINT('',(1.97,-2.35,2.4));
#21113=CARTESIAN_POINT('',(1.97,-2.35,2.4));
#21114=CARTESIAN_POINT('',(0.,-2.35,2.4));
#21115=CARTESIAN_POINT('Origin',(0.,2.35,2.4));
#21116=CARTESIAN_POINT('',(1.97,2.35,2.4));
#21117=CARTESIAN_POINT('',(1.97,2.35,2.4));
#21118=CARTESIAN_POINT('',(0.,2.35,2.4));
#21119=CARTESIAN_POINT('Origin',(0.,2.35,1.75));
#21120=CARTESIAN_POINT('',(1.97,2.35,1.75));
#21121=CARTESIAN_POINT('',(1.97,2.35,1.75));
#21122=CARTESIAN_POINT('',(0.,2.35,1.75));
#21123=CARTESIAN_POINT('Origin',(0.,1.7,1.75));
#21124=CARTESIAN_POINT('',(1.97,1.7,1.75));
#21125=CARTESIAN_POINT('Origin',(0.,0.78,0.43));
#21126=CARTESIAN_POINT('',(1.97,0.78,0.43));
#21127=CARTESIAN_POINT('',(1.97,0.78,0.43));
#21128=CARTESIAN_POINT('',(0.,0.78,0.43));
#21129=CARTESIAN_POINT('Origin',(0.,0.78,1.55));
#21130=CARTESIAN_POINT('',(1.97,0.78,1.55));
#21131=CARTESIAN_POINT('',(1.97,0.78,1.55));
#21132=CARTESIAN_POINT('',(0.,0.78,1.55));
#21133=CARTESIAN_POINT('Origin',(0.,-0.78,1.55));
#21134=CARTESIAN_POINT('',(1.97,-0.78,1.55));
#21135=CARTESIAN_POINT('',(1.97,-0.78,1.55));
#21136=CARTESIAN_POINT('',(0.,-0.78,1.55));
#21137=CARTESIAN_POINT('Origin',(0.,-0.78,0.43));
#21138=CARTESIAN_POINT('',(1.97,-0.78,0.43));
#21139=CARTESIAN_POINT('',(1.97,-0.78,0.43));
#21140=CARTESIAN_POINT('',(0.,-0.78,0.43));
#21141=CARTESIAN_POINT('Origin',(0.,-1.7,0.43));
#21142=CARTESIAN_POINT('',(1.97,-1.7,0.43));
#21143=CARTESIAN_POINT('Origin',(1.97,0.,1.415));
#21144=CARTESIAN_POINT('',(0.,0.,0.));
#21145=CARTESIAN_POINT('Origin',(1.97,1.7,2.3));
#21146=CARTESIAN_POINT('',(1.97,1.7,2.3));
#21147=CARTESIAN_POINT('',(1.97,-1.7,2.3));
#21148=CARTESIAN_POINT('',(1.97,1.7,2.3));
#21149=CARTESIAN_POINT('',(3.07,-1.7,2.3));
#21150=CARTESIAN_POINT('',(1.97,-1.7,2.3));
#21151=CARTESIAN_POINT('',(3.07,1.7,2.3));
#21152=CARTESIAN_POINT('',(3.07,1.7,2.3));
#21153=CARTESIAN_POINT('',(1.97,1.7,2.3));
#21154=CARTESIAN_POINT('Origin',(1.97,1.7,0.46));
#21155=CARTESIAN_POINT('',(1.97,1.7,0.46));
#21156=CARTESIAN_POINT('',(1.97,1.7,0.46));
#21157=CARTESIAN_POINT('',(3.07,1.7,0.46));
#21158=CARTESIAN_POINT('',(3.07,1.7,0.46));
#21159=CARTESIAN_POINT('',(1.97,1.7,0.46));
#21160=CARTESIAN_POINT('Origin',(1.97,0.78,0.46));
#21161=CARTESIAN_POINT('',(1.97,0.78,0.46));
#21162=CARTESIAN_POINT('',(1.97,0.78,0.46));
#21163=CARTESIAN_POINT('',(3.07,0.78,0.46));
#21164=CARTESIAN_POINT('',(3.07,0.78,0.46));
#21165=CARTESIAN_POINT('',(1.97,0.78,0.46));
#21166=CARTESIAN_POINT('Origin',(1.97,0.78,1.55));
#21167=CARTESIAN_POINT('',(1.97,0.78,1.55));
#21168=CARTESIAN_POINT('',(1.97,0.78,1.55));
#21169=CARTESIAN_POINT('',(3.07,0.78,1.55));
#21170=CARTESIAN_POINT('',(3.07,0.78,1.55));
#21171=CARTESIAN_POINT('',(1.97,0.78,1.55));
#21172=CARTESIAN_POINT('Origin',(1.97,-0.78,1.55));
#21173=CARTESIAN_POINT('',(1.97,-0.78,1.55));
#21174=CARTESIAN_POINT('',(1.97,-0.78,1.55));
#21175=CARTESIAN_POINT('',(3.07,-0.78,1.55));
#21176=CARTESIAN_POINT('',(3.07,-0.78,1.55));
#21177=CARTESIAN_POINT('',(1.97,-0.78,1.55));
#21178=CARTESIAN_POINT('Origin',(1.97,-0.78,0.46));
#21179=CARTESIAN_POINT('',(1.97,-0.78,0.46));
#21180=CARTESIAN_POINT('',(1.97,-0.78,0.46));
#21181=CARTESIAN_POINT('',(3.07,-0.78,0.46));
#21182=CARTESIAN_POINT('',(3.07,-0.78,0.46));
#21183=CARTESIAN_POINT('',(1.97,-0.78,0.46));
#21184=CARTESIAN_POINT('Origin',(1.97,-1.7,0.46));
#21185=CARTESIAN_POINT('',(1.97,-1.7,0.46));
#21186=CARTESIAN_POINT('',(1.97,-1.7,0.46));
#21187=CARTESIAN_POINT('',(3.07,-1.7,0.46));
#21188=CARTESIAN_POINT('',(3.07,-1.7,0.46));
#21189=CARTESIAN_POINT('',(1.97,-1.7,0.46));
#21190=CARTESIAN_POINT('Origin',(1.97,-1.7,2.3));
#21191=CARTESIAN_POINT('',(1.97,-1.7,2.3));
#21192=CARTESIAN_POINT('',(3.07,-1.7,2.3));
#21193=CARTESIAN_POINT('Origin',(3.07,0.,1.38));
#21194=CARTESIAN_POINT('Origin',(1.97,0.,1.38));
#21195=CARTESIAN_POINT('',(0.,0.,0.));
#21196=CARTESIAN_POINT('Origin',(-1.97,-0.78,0.46));
#21197=CARTESIAN_POINT('',(-1.97,-1.7,0.46));
#21198=CARTESIAN_POINT('',(-1.97,-0.78,0.46));
#21199=CARTESIAN_POINT('',(-1.97,-1.7,0.46));
#21200=CARTESIAN_POINT('',(-3.07,-1.7,0.46));
#21201=CARTESIAN_POINT('',(-1.97,-1.7,0.46));
#21202=CARTESIAN_POINT('',(-3.07,-0.78,0.46));
#21203=CARTESIAN_POINT('',(-3.07,-1.7,0.46));
#21204=CARTESIAN_POINT('',(-1.97,-0.78,0.46));
#21205=CARTESIAN_POINT('Origin',(-1.97,-0.78,1.55));
#21206=CARTESIAN_POINT('',(-1.97,-0.78,1.55));
#21207=CARTESIAN_POINT('',(-1.97,-0.78,0.46));
#21208=CARTESIAN_POINT('',(-3.07,-0.78,1.55));
#21209=CARTESIAN_POINT('',(-3.07,-0.78,0.46));
#21210=CARTESIAN_POINT('',(-1.97,-0.78,1.55));
#21211=CARTESIAN_POINT('Origin',(-1.97,0.78,1.55));
#21212=CARTESIAN_POINT('',(-1.97,0.78,1.55));
#21213=CARTESIAN_POINT('',(-1.97,-0.78,1.55));
#21214=CARTESIAN_POINT('',(-3.07,0.78,1.55));
#21215=CARTESIAN_POINT('',(-3.07,-0.78,1.55));
#21216=CARTESIAN_POINT('',(-1.97,0.78,1.55));
#21217=CARTESIAN_POINT('Origin',(-1.97,0.78,0.46));
#21218=CARTESIAN_POINT('',(-1.97,0.78,0.46));
#21219=CARTESIAN_POINT('',(-1.97,0.78,1.55));
#21220=CARTESIAN_POINT('',(-3.07,0.78,0.46));
#21221=CARTESIAN_POINT('',(-3.07,0.78,1.55));
#21222=CARTESIAN_POINT('',(-1.97,0.78,0.46));
#21223=CARTESIAN_POINT('Origin',(-1.97,1.7,0.46));
#21224=CARTESIAN_POINT('',(-1.97,1.7,0.46));
#21225=CARTESIAN_POINT('',(-1.97,0.78,0.46));
#21226=CARTESIAN_POINT('',(-3.07,1.7,0.46));
#21227=CARTESIAN_POINT('',(-3.07,0.78,0.46));
#21228=CARTESIAN_POINT('',(-1.97,1.7,0.46));
#21229=CARTESIAN_POINT('Origin',(-1.97,1.7,2.3));
#21230=CARTESIAN_POINT('',(-1.97,1.7,2.3));
#21231=CARTESIAN_POINT('',(-1.97,1.7,0.46));
#21232=CARTESIAN_POINT('',(-3.07,1.7,2.3));
#21233=CARTESIAN_POINT('',(-3.07,1.7,0.46));
#21234=CARTESIAN_POINT('',(-1.97,1.7,2.3));
#21235=CARTESIAN_POINT('Origin',(-1.97,-1.7,2.3));
#21236=CARTESIAN_POINT('',(-1.97,-1.7,2.3));
#21237=CARTESIAN_POINT('',(-1.97,1.7,2.3));
#21238=CARTESIAN_POINT('',(-3.07,-1.7,2.3));
#21239=CARTESIAN_POINT('',(-3.07,1.7,2.3));
#21240=CARTESIAN_POINT('',(-1.97,-1.7,2.3));
#21241=CARTESIAN_POINT('Origin',(-1.97,-1.7,0.46));
#21242=CARTESIAN_POINT('',(-1.97,-1.7,2.3));
#21243=CARTESIAN_POINT('',(-3.07,-1.7,2.3));
#21244=CARTESIAN_POINT('Origin',(-1.97,0.,1.38));
#21245=CARTESIAN_POINT('Origin',(-3.07,0.,1.38));
#21246=CARTESIAN_POINT('',(0.,0.,0.));
#21247=CARTESIAN_POINT('',(0.,0.,0.));
#21248=CARTESIAN_POINT('',(0.,0.,0.));
#21249=CARTESIAN_POINT('',(0.,0.,0.));
#21250=CARTESIAN_POINT('Origin',(0.,0.09,0.));
#21251=CARTESIAN_POINT('',(-0.285,0.1,3.49024337756996E-17));
#21252=CARTESIAN_POINT('Origin',(0.,0.1,0.));
#21253=CARTESIAN_POINT('',(-0.265,0.08,-3.24531401774049E-17));
#21254=CARTESIAN_POINT('',(-0.275,0.09,3.36777869765522E-17));
#21255=CARTESIAN_POINT('Origin',(0.,0.08,0.));
#21256=CARTESIAN_POINT('Origin',(0.,0.,0.));
#21257=CARTESIAN_POINT('',(-0.265,0.,3.24531401774049E-17));
#21258=CARTESIAN_POINT('',(-0.265,0.,3.24531401774049E-17));
#21259=CARTESIAN_POINT('Origin',(0.,0.,0.));
#21260=CARTESIAN_POINT('Origin',(0.,0.1,0.));
#21261=CARTESIAN_POINT('',(-0.5,0.1,6.12323399573677E-17));
#21262=CARTESIAN_POINT('Origin',(0.,0.1,0.));
#21263=CARTESIAN_POINT('Origin',(0.,0.,0.));
#21264=CARTESIAN_POINT('',(-0.5,0.,6.12323399573677E-17));
#21265=CARTESIAN_POINT('',(-0.5,0.,6.12323399573677E-17));
#21266=CARTESIAN_POINT('Origin',(0.,0.,0.));
#21267=CARTESIAN_POINT('Origin',(0.,0.,0.));
#21268=CARTESIAN_POINT('',(0.,0.,0.));
#21269=CARTESIAN_POINT('Origin',(0.115470053837925,-0.5,-0.2));
#21270=CARTESIAN_POINT('',(0.23094010767585,-0.5,0.));
#21271=CARTESIAN_POINT('',(0.115470053837925,-0.5,-0.2));
#21272=CARTESIAN_POINT('',(0.23094010767585,-0.5,0.));
#21273=CARTESIAN_POINT('',(0.115470053837925,-0.8,-0.2));
#21274=CARTESIAN_POINT('',(0.115470053837925,-0.5,-0.2));
#21275=CARTESIAN_POINT('',(0.23094010767585,-0.8,0.));
#21276=CARTESIAN_POINT('',(0.23094010767585,-0.8,0.));
#21277=CARTESIAN_POINT('',(0.23094010767585,-0.5,0.));
#21278=CARTESIAN_POINT('Origin',(-0.115470053837925,-0.5,-0.2));
#21279=CARTESIAN_POINT('',(-0.115470053837925,-0.5,-0.2));
#21280=CARTESIAN_POINT('',(0.115470053837925,-0.5,-0.2));
#21281=CARTESIAN_POINT('',(-0.115470053837925,-0.8,-0.2));
#21282=CARTESIAN_POINT('',(-0.115470053837925,-0.5,-0.2));
#21283=CARTESIAN_POINT('',(0.115470053837925,-0.8,-0.2));
#21284=CARTESIAN_POINT('Origin',(-0.23094010767585,-0.5,-2.77555756156289E-17));
#21285=CARTESIAN_POINT('',(-0.23094010767585,-0.5,-2.82820063659975E-17));
#21286=CARTESIAN_POINT('',(-0.115470053837925,-0.5,-0.2));
#21287=CARTESIAN_POINT('',(-0.23094010767585,-0.8,-2.77555756156289E-17));
#21288=CARTESIAN_POINT('',(-0.23094010767585,-0.5,-2.82820063659975E-17));
#21289=CARTESIAN_POINT('',(-0.115470053837925,-0.8,-0.2));
#21290=CARTESIAN_POINT('Origin',(-0.115470053837925,-0.5,0.2));
#21291=CARTESIAN_POINT('',(-0.115470053837925,-0.5,0.2));
#21292=CARTESIAN_POINT('',(-0.23094010767585,-0.5,-2.82820063659975E-17));
#21293=CARTESIAN_POINT('',(-0.115470053837925,-0.8,0.2));
#21294=CARTESIAN_POINT('',(-0.115470053837925,-0.5,0.2));
#21295=CARTESIAN_POINT('',(-0.23094010767585,-0.8,-2.82820063659975E-17));
#21296=CARTESIAN_POINT('Origin',(0.115470053837925,-0.5,0.2));
#21297=CARTESIAN_POINT('',(0.115470053837925,-0.5,0.2));
#21298=CARTESIAN_POINT('',(-0.115470053837925,-0.5,0.2));
#21299=CARTESIAN_POINT('',(0.115470053837925,-0.8,0.2));
#21300=CARTESIAN_POINT('',(0.115470053837925,-0.5,0.2));
#21301=CARTESIAN_POINT('',(-0.115470053837925,-0.8,0.2));
#21302=CARTESIAN_POINT('Origin',(0.23094010767585,-0.5,0.));
#21303=CARTESIAN_POINT('',(0.115470053837925,-0.5,0.2));
#21304=CARTESIAN_POINT('',(0.115470053837925,-0.8,0.2));
#21305=CARTESIAN_POINT('Origin',(0.,-0.5,0.));
#21306=CARTESIAN_POINT('Origin',(0.,-0.8,0.));
#21307=CARTESIAN_POINT('Origin',(0.,-1.9,0.));
#21308=CARTESIAN_POINT('',(-0.25,-1.9,3.06161699786838E-17));
#21309=CARTESIAN_POINT('Origin',(0.,-1.9,0.));
#21310=CARTESIAN_POINT('',(-0.24505,-1.9,3.00099698131059E-17));
#21311=CARTESIAN_POINT('Origin',(0.,-1.9,0.));
#21312=CARTESIAN_POINT('Origin',(0.,-3.,0.));
#21313=CARTESIAN_POINT('',(-0.25,-3.,3.06161699786838E-17));
#21314=CARTESIAN_POINT('',(-0.25,-3.,3.06161699786838E-17));
#21315=CARTESIAN_POINT('Origin',(0.,-3.,0.));
#21316=CARTESIAN_POINT('Origin',(0.,-3.,0.));
#21317=CARTESIAN_POINT('Origin',(0.375,0.5,0.));
#21318=CARTESIAN_POINT('',(-0.375,0.5,-4.59242549680257E-17));
#21319=CARTESIAN_POINT('Origin',(0.,0.5,0.));
#21320=CARTESIAN_POINT('Origin',(0.,0.475,0.));
#21321=CARTESIAN_POINT('',(-0.425,0.45,-5.20474889637625E-17));
#21322=CARTESIAN_POINT('Origin',(0.,0.45,0.));
#21323=CARTESIAN_POINT('',(-0.4,0.475,-4.89858719658941E-17));
#21324=CARTESIAN_POINT('Origin',(0.,0.24,0.));
#21325=CARTESIAN_POINT('',(-0.425,0.0299999999999998,-5.20474889637625E-17));
#21326=CARTESIAN_POINT('Origin',(0.,0.0299999999999998,0.));
#21327=CARTESIAN_POINT('',(-0.425,0.24,-5.20474889637625E-17));
#21328=CARTESIAN_POINT('Origin',(0.,0.0150000000000001,0.));
#21329=CARTESIAN_POINT('',(-0.395,4.85722573273506E-17,-4.83735485663204E-17));
#21330=CARTESIAN_POINT('Origin',(0.,0.,0.));
#21331=CARTESIAN_POINT('',(-0.41,0.0150000000000001,-5.02105187650415E-17));
#21332=CARTESIAN_POINT('Origin',(0.27,0.,0.));
#21333=CARTESIAN_POINT('',(-0.27,0.,-3.30654635769785E-17));
#21334=CARTESIAN_POINT('Origin',(0.,0.,0.));
#21335=CARTESIAN_POINT('Origin',(0.,-0.02,0.));
#21336=CARTESIAN_POINT('',(-0.24505,-0.0498999999999999,3.00099698131059E-17));
#21337=CARTESIAN_POINT('Origin',(0.,-0.0498999999999999,0.));
#21338=CARTESIAN_POINT('',(-0.26,-0.02,-3.18408167778312E-17));
#21339=CARTESIAN_POINT('Origin',(0.,-0.995,0.));
#21340=CARTESIAN_POINT('',(-0.24505,-0.995,-3.00099698131059E-17));
#21341=CARTESIAN_POINT('',(0.,0.,0.));
#21342=CARTESIAN_POINT('Origin',(12.5,0.,4.));
#21343=CARTESIAN_POINT('',(12.7800042915148,-1.13874042544416E-5,4.45787212683272));
#21344=CARTESIAN_POINT('',(12.6699957084852,1.09516003635735E-5,4.45788309353564));
#21345=CARTESIAN_POINT('',(12.5,-5.60735153159594E-17,4.457875));
#21346=CARTESIAN_POINT('',(12.5,-0.186196943290586,3.58169363627331));
#21347=CARTESIAN_POINT('Ctrl Pts',(12.6699957084852,1.09516003635735E-5,
4.45788309353564));
#21348=CARTESIAN_POINT('Ctrl Pts',(12.6684300766731,0.0150239422001319,
4.45789815019349));
#21349=CARTESIAN_POINT('Ctrl Pts',(12.6668644448611,0.0300354905662504,
4.45717403092565));
#21350=CARTESIAN_POINT('Ctrl Pts',(12.6652988130491,0.0449730203321769,
4.45569984746698));
#21351=CARTESIAN_POINT('Ctrl Pts',(12.6574274409991,0.120072959788606,4.44828824124903));
#21352=CARTESIAN_POINT('Ctrl Pts',(12.6495560689492,0.193301947984492,4.42191743369942));
#21353=CARTESIAN_POINT('Ctrl Pts',(12.6416846968992,0.255884660534875,4.37974732787395));
#21354=CARTESIAN_POINT('Ctrl Pts',(12.6338133248492,0.318467373085258,4.33757722204849));
#21355=CARTESIAN_POINT('Ctrl Pts',(12.6259419527993,0.370403809990138,4.27960781794716));
#21356=CARTESIAN_POINT('Ctrl Pts',(12.6180705807493,0.405471379329245,4.2127856577826));
#21357=CARTESIAN_POINT('Ctrl Pts',(12.6101992086994,0.440538948668352,4.14596349761803));
#21358=CARTESIAN_POINT('Ctrl Pts',(12.6023278366494,0.458737650441686,4.07028858139023));
#21359=CARTESIAN_POINT('Ctrl Pts',(12.5944564645995,0.457884906392306,3.99482861029462));
#21360=CARTESIAN_POINT('Ctrl Pts',(12.5865850925495,0.457032162342926,3.91936863919901));
#21361=CARTESIAN_POINT('Ctrl Pts',(12.5787137204996,0.437127972470831,3.84412361323559));
#21362=CARTESIAN_POINT('Ctrl Pts',(12.5708423484496,0.400561475243013,3.77811083326841));
#21363=CARTESIAN_POINT('Ctrl Pts',(12.5629709763996,0.363994978015195,3.71209805330123));
#21364=CARTESIAN_POINT('Ctrl Pts',(12.5550996043497,0.310766173431653,3.6553175193303));
#21365=CARTESIAN_POINT('Ctrl Pts',(12.5472282322997,0.247245050961511,3.61457214242492));
#21366=CARTESIAN_POINT('Ctrl Pts',(12.5393568602498,0.183723928491369,3.57382676551955));
#21367=CARTESIAN_POINT('Ctrl Pts',(12.5314854881998,0.109910488134627,3.54911654567973));
#21368=CARTESIAN_POINT('Ctrl Pts',(12.5236141161499,0.034670519197381,3.5434092666393));
#21369=CARTESIAN_POINT('Ctrl Pts',(12.5157427440999,-0.0405694497398647,
3.53770198759887));
#21370=CARTESIAN_POINT('Ctrl Pts',(12.50787137205,-0.117235947257613,3.55099764935784));
#21371=CARTESIAN_POINT('Ctrl Pts',(12.5,-0.186196943290592,3.58169363627332));
#21372=CARTESIAN_POINT('',(12.5,-0.186217277007329,4.41832740439831));
#21373=CARTESIAN_POINT('Origin',(12.5,0.,4.));
#21374=CARTESIAN_POINT('Ctrl Pts',(12.5,-0.186217277007329,4.41832740439831));
#21375=CARTESIAN_POINT('Ctrl Pts',(12.5008157411716,-0.193365324225124,
4.41515241707318));
#21376=CARTESIAN_POINT('Ctrl Pts',(12.5016314823431,-0.200430783441492,
4.4117927098014));
#21377=CARTESIAN_POINT('Ctrl Pts',(12.5024472235147,-0.207403505574881,
4.40825058102053));
#21378=CARTESIAN_POINT('Ctrl Pts',(12.5103185955646,-0.274685741688951,
4.37407134077235));
#21379=CARTESIAN_POINT('Ctrl Pts',(12.5181899676146,-0.333333232193243,
4.32290684204764));
#21380=CARTESIAN_POINT('Ctrl Pts',(12.5260613396645,-0.376326743005614,
4.26088786252735));
#21381=CARTESIAN_POINT('Ctrl Pts',(12.5339327117145,-0.419320253817985,
4.19886888300706));
#21382=CARTESIAN_POINT('Ctrl Pts',(12.5418040837645,-0.446659784938435,
4.12599542269119));
#21383=CARTESIAN_POINT('Ctrl Pts',(12.5496754558144,-0.455065168373522,
4.05100019606997));
#21384=CARTESIAN_POINT('Ctrl Pts',(12.5575468278644,-0.463470551808608,
3.97600496944875));
#21385=CARTESIAN_POINT('Ctrl Pts',(12.5654181999143,-0.452941787558331,
3.89888797652218));
#21386=CARTESIAN_POINT('Ctrl Pts',(12.5732895719643,-0.424742400952558,
3.82888990513641));
#21387=CARTESIAN_POINT('Ctrl Pts',(12.5811609440142,-0.396543014346786,
3.75889183375065));
#21388=CARTESIAN_POINT('Ctrl Pts',(12.5890323160642,-0.350673005385519,
3.69601268390568));
#21389=CARTESIAN_POINT('Ctrl Pts',(12.5969036881141,-0.292628022669152,
3.64778723809593));
#21390=CARTESIAN_POINT('Ctrl Pts',(12.6047750601641,-0.234583039952784,
3.59956179228618));
#21391=CARTESIAN_POINT('Ctrl Pts',(12.6126464322141,-0.164363083481316,
3.56599005051166));
#21392=CARTESIAN_POINT('Ctrl Pts',(12.620517804264,-0.0903829156297007,
3.55109483330951));
#21393=CARTESIAN_POINT('Ctrl Pts',(12.628389176314,-0.0164027477780855,
3.53619961610736));
#21394=CARTESIAN_POINT('Ctrl Pts',(12.6362605483639,0.0613376314536766,
3.53998092347757));
#21395=CARTESIAN_POINT('Ctrl Pts',(12.6441319204139,0.13352290298843,3.56198566164487));
#21396=CARTESIAN_POINT('Ctrl Pts',(12.6520032924638,0.205708174523184,3.58399039981218));
#21397=CARTESIAN_POINT('Ctrl Pts',(12.6598746645138,0.272338338360929,3.62421856877658));
#21398=CARTESIAN_POINT('Ctrl Pts',(12.6677460365637,0.325429113408527,3.67784968145944));
#21399=CARTESIAN_POINT('Ctrl Pts',(12.6756174086137,0.378519888456125,3.7314807941423));
#21400=CARTESIAN_POINT('Ctrl Pts',(12.6834887806637,0.418071274713577,3.79851485054363));
#21401=CARTESIAN_POINT('Ctrl Pts',(12.6913601527136,0.439343931585728,3.87091926467948));
#21402=CARTESIAN_POINT('Ctrl Pts',(12.6992315247636,0.460616588457879,3.94332367881533));
#21403=CARTESIAN_POINT('Ctrl Pts',(12.7071028968135,0.46361051594473,4.02109845068571));
#21404=CARTESIAN_POINT('Ctrl Pts',(12.7149742688635,0.447966936692366,4.09492394607626));
#21405=CARTESIAN_POINT('Ctrl Pts',(12.7228456409134,0.432323357440003,4.16874944146681));
#21406=CARTESIAN_POINT('Ctrl Pts',(12.7307170129634,0.398042271448426,4.23862566037754));
#21407=CARTESIAN_POINT('Ctrl Pts',(12.7385883850133,0.349231538304918,4.29617944234672));
#21408=CARTESIAN_POINT('Ctrl Pts',(12.7464597570633,0.300420805161409,4.35373322431589));
#21409=CARTESIAN_POINT('Ctrl Pts',(12.7543311291133,0.237080424865968,4.39896456934351));
#21410=CARTESIAN_POINT('Ctrl Pts',(12.7622025011632,0.166800374688878,4.42645347375649));
#21411=CARTESIAN_POINT('Ctrl Pts',(12.7681364312804,0.113818899065861,4.4471763206439));
#21412=CARTESIAN_POINT('Ctrl Pts',(12.7740703613976,0.056893551674301,4.45781599184163));
#21413=CARTESIAN_POINT('Ctrl Pts',(12.7800042915148,-1.13874042544416E-5,
4.45787212683272));
#21414=CARTESIAN_POINT('Origin',(12.5,0.,4.));
#21415=CARTESIAN_POINT('',(13.0800042915148,2.8196954984682E-6,4.45783894202495));
#21416=CARTESIAN_POINT('',(12.9699957084852,-6.90274666573233E-6,4.45790451736119));
#21417=CARTESIAN_POINT('',(12.5,-5.60735153159594E-17,4.457875));
#21418=CARTESIAN_POINT('Ctrl Pts',(12.9699957084852,-6.90274666573233E-6,
4.45790451736119));
#21419=CARTESIAN_POINT('Ctrl Pts',(12.9628865412726,0.0681543496286777,
4.45785453236543));
#21420=CARTESIAN_POINT('Ctrl Pts',(12.95577737406,0.136337475731944,4.44242789501186));
#21421=CARTESIAN_POINT('Ctrl Pts',(12.9486682068475,0.197807532932104,4.41298560914613));
#21422=CARTESIAN_POINT('Ctrl Pts',(12.9407968347975,0.265868063186489,4.38038668734267));
#21423=CARTESIAN_POINT('Ctrl Pts',(12.9329254627476,0.325698883531032,4.33060565060516));
#21424=CARTESIAN_POINT('Ctrl Pts',(12.9250540906976,0.370130557623211,4.26960768492436));
#21425=CARTESIAN_POINT('Ctrl Pts',(12.9171827186476,0.41456223171539,4.20860971924356));
#21426=CARTESIAN_POINT('Ctrl Pts',(12.9093113465977,0.443594759555206,4.13639482461947));
#21427=CARTESIAN_POINT('Ctrl Pts',(12.9014399745477,0.453749217534713,4.06161640217293));
#21428=CARTESIAN_POINT('Ctrl Pts',(12.8935686024978,0.463903675514219,3.9868379797264));
#21429=CARTESIAN_POINT('Ctrl Pts',(12.8856972304478,0.455180063633418,3.90949602945742));
#21430=CARTESIAN_POINT('Ctrl Pts',(12.8778258583979,0.428623718850503,3.83885831972366));
#21431=CARTESIAN_POINT('Ctrl Pts',(12.8699544863479,0.402067374067587,3.7682206099899));
#21432=CARTESIAN_POINT('Ctrl Pts',(12.862083114298,0.357678296382559,3.70428714079136));
#21433=CARTESIAN_POINT('Ctrl Pts',(12.854211742248,0.300775561959983,3.65471896268111));
#21434=CARTESIAN_POINT('Ctrl Pts',(12.846340370198,0.243872827537407,3.60515078457087));
#21435=CARTESIAN_POINT('Ctrl Pts',(12.8384689981481,0.174456436377283,3.56994789754891));
#21436=CARTESIAN_POINT('Ctrl Pts',(12.8305976260981,0.100844448250471,3.55332860992135));
#21437=CARTESIAN_POINT('Ctrl Pts',(12.8227262540482,0.0272324601236582,
3.53670932229378));
#21438=CARTESIAN_POINT('Ctrl Pts',(12.8148548819982,-0.0505751249698428,
3.53867363406062));
#21439=CARTESIAN_POINT('Ctrl Pts',(12.8069835099483,-0.123254740362562,
3.558986165072));
#21440=CARTESIAN_POINT('Ctrl Pts',(12.7991121378983,-0.195934355755281,
3.57929869608338));
#21441=CARTESIAN_POINT('Ctrl Pts',(12.7912407658484,-0.263486001447217,
3.6179594463393));
#21442=CARTESIAN_POINT('Ctrl Pts',(12.7833693937984,-0.317815070570116,
3.67033575613656));
#21443=CARTESIAN_POINT('Ctrl Pts',(12.7754980217484,-0.372144139693014,
3.72271206593382));
#21444=CARTESIAN_POINT('Ctrl Pts',(12.7676266496985,-0.413250632246875,
3.78880393527241));
#21445=CARTESIAN_POINT('Ctrl Pts',(12.7597552776485,-0.43620881068128,3.86069167744737));
#21446=CARTESIAN_POINT('Ctrl Pts',(12.7518839055986,-0.459166989115684,
3.93257941962233));
#21447=CARTESIAN_POINT('Ctrl Pts',(12.7440125335486,-0.463976853430633,
4.01026303463365));
#21448=CARTESIAN_POINT('Ctrl Pts',(12.7361411614987,-0.450062064178823,
4.08443380953254));
#21449=CARTESIAN_POINT('Ctrl Pts',(12.7282697894487,-0.436147274927012,
4.15860458443143));
#21450=CARTESIAN_POINT('Ctrl Pts',(12.7203984173988,-0.403507832108441,
4.22926251921788));
#21451=CARTESIAN_POINT('Ctrl Pts',(12.7125270453488,-0.356054829243877,
4.28794078818664));
#21452=CARTESIAN_POINT('Ctrl Pts',(12.7046556732988,-0.308601826379312,
4.3466190571554));
#21453=CARTESIAN_POINT('Ctrl Pts',(12.6967843012489,-0.246335263468753,
4.39331766030646));
#21454=CARTESIAN_POINT('Ctrl Pts',(12.6889129291989,-0.176716536654988,
4.42244075943884));
#21455=CARTESIAN_POINT('Ctrl Pts',(12.682607188961,-0.120945115332726,4.44577121528397));
#21456=CARTESIAN_POINT('Ctrl Pts',(12.6763014487231,-0.0604553842193124,
4.45782245132557));
#21457=CARTESIAN_POINT('Ctrl Pts',(12.6699957084852,1.09516003635735E-5,
4.45788309353564));
#21458=CARTESIAN_POINT('Ctrl Pts',(12.7800042915148,-1.13874042544416E-5,
4.45787212683272));
#21459=CARTESIAN_POINT('Ctrl Pts',(12.7819417334476,-0.0185909818676029,
4.45789045503738));
#21460=CARTESIAN_POINT('Ctrl Pts',(12.7838791753803,-0.0371684007279871,
4.45678053845584));
#21461=CARTESIAN_POINT('Ctrl Pts',(12.7858166173131,-0.0556056617636943,
4.45452496135198));
#21462=CARTESIAN_POINT('Ctrl Pts',(12.793687989363,-0.130511927980435,4.44536108073615));
#21463=CARTESIAN_POINT('Ctrl Pts',(12.801559361413,-0.203104740355178,4.41728685570614));
#21464=CARTESIAN_POINT('Ctrl Pts',(12.8094307334629,-0.264685413403174,
4.37366637792357));
#21465=CARTESIAN_POINT('Ctrl Pts',(12.8173021055129,-0.32626608645117,4.33004590014099));
#21466=CARTESIAN_POINT('Ctrl Pts',(12.8251734775629,-0.37683462017242,4.27087916960585));
#21467=CARTESIAN_POINT('Ctrl Pts',(12.8330448496128,-0.410331463567461,
4.20325604577686));
#21468=CARTESIAN_POINT('Ctrl Pts',(12.8409162216628,-0.443828306962503,
4.13563292194788));
#21469=CARTESIAN_POINT('Ctrl Pts',(12.8487875937127,-0.460253460031337,
4.05955340482505));
#21470=CARTESIAN_POINT('Ctrl Pts',(12.8566589657627,-0.457638721839564,
3.98413398734005));
#21471=CARTESIAN_POINT('Ctrl Pts',(12.8645303378126,-0.45502398364779,3.90871456985506));
#21472=CARTESIAN_POINT('Ctrl Pts',(12.8724017098626,-0.433369354195409,
3.8339552520079));
#21473=CARTESIAN_POINT('Ctrl Pts',(12.8802730819125,-0.395269674734573,
3.76881432927916));
#21474=CARTESIAN_POINT('Ctrl Pts',(12.8881444539625,-0.357169995273737,
3.70367340655041));
#21475=CARTESIAN_POINT('Ctrl Pts',(12.8960158260125,-0.302625265804445,
3.64815087894007));
#21476=CARTESIAN_POINT('Ctrl Pts',(12.9038871980624,-0.238171498431664,
3.6088999265713));
#21477=CARTESIAN_POINT('Ctrl Pts',(12.9117585701124,-0.173717731058884,
3.56964897420252));
#21478=CARTESIAN_POINT('Ctrl Pts',(12.9196299421623,-0.0993549257826154,
3.5466695970753));
#21479=CARTESIAN_POINT('Ctrl Pts',(12.9275013142123,-0.023993864556795,
3.54271537903906));
#21480=CARTESIAN_POINT('Ctrl Pts',(12.9353726862622,0.0513671966690251,
3.53876116100282));
#21481=CARTESIAN_POINT('Ctrl Pts',(12.9432440583122,0.127726513844396,3.55383210205756));
#21482=CARTESIAN_POINT('Ctrl Pts',(12.9511154303621,0.195934065997641,3.58612227423372));
#21483=CARTESIAN_POINT('Ctrl Pts',(12.9589868024121,0.264141618150887,3.61841244640988));
#21484=CARTESIAN_POINT('Ctrl Pts',(12.9668581744621,0.324197405282005,3.66792184970745));
#21485=CARTESIAN_POINT('Ctrl Pts',(12.974729546512,0.368905033668178,3.72871784755079));
#21486=CARTESIAN_POINT('Ctrl Pts',(12.982600918562,0.41361266205435,3.78951384539413));
#21487=CARTESIAN_POINT('Ctrl Pts',(12.9904722906119,0.442972131695578,3.86159643778324));
#21488=CARTESIAN_POINT('Ctrl Pts',(12.9983436626619,0.453465341949404,3.93632807718928));
#21489=CARTESIAN_POINT('Ctrl Pts',(13.0062150347118,0.46395855220323,4.01105971659532));
#21490=CARTESIAN_POINT('Ctrl Pts',(13.0140864067618,0.455585503069655,4.0884404030183));
#21491=CARTESIAN_POINT('Ctrl Pts',(13.0219577788117,0.429349524305901,4.15919772637108));
#21492=CARTESIAN_POINT('Ctrl Pts',(13.0298291508617,0.403113545542148,4.22995504972387));
#21493=CARTESIAN_POINT('Ctrl Pts',(13.0377005229117,0.359014637148215,4.29408901000646));
#21494=CARTESIAN_POINT('Ctrl Pts',(13.0455718949616,0.302337104315659,4.34391453219887));
#21495=CARTESIAN_POINT('Ctrl Pts',(13.0534432670116,0.245659571483104,4.39374005439127));
#21496=CARTESIAN_POINT('Ctrl Pts',(13.0613146390615,0.176403414211925,4.4292571384935));
#21497=CARTESIAN_POINT('Ctrl Pts',(13.0691860111115,0.102867492605122,4.44620982627979));
#21498=CARTESIAN_POINT('Ctrl Pts',(13.0727921045793,0.0691786509558273,
4.45397632191734));
#21499=CARTESIAN_POINT('Ctrl Pts',(13.076398198047,0.0345915681853763,4.45784650391406));
#21500=CARTESIAN_POINT('Ctrl Pts',(13.0800042915148,2.8196954984682E-6,
4.45783894202495));
#21501=CARTESIAN_POINT('Origin',(12.5,0.,4.));
#21502=CARTESIAN_POINT('',(13.3800042915148,1.00338821889499E-5,4.45789143379912));
#21503=CARTESIAN_POINT('',(13.2699957084852,-6.83105689078257E-6,4.45784477598907));
#21504=CARTESIAN_POINT('',(12.5,-5.60735153159594E-17,4.457875));
#21505=CARTESIAN_POINT('Ctrl Pts',(13.2699957084852,-6.83105689078257E-6,
4.45784477598907));
#21506=CARTESIAN_POINT('Ctrl Pts',(13.265214377922,0.0458528260712244,4.45782008288951));
#21507=CARTESIAN_POINT('Ctrl Pts',(13.2604330473589,0.091719698604501,4.45096974854549));
#21508=CARTESIAN_POINT('Ctrl Pts',(13.2556517167957,0.135506404234727,4.43740478719402));
#21509=CARTESIAN_POINT('Ctrl Pts',(13.2477803447458,0.207591244700251,4.41507316710824));
#21510=CARTESIAN_POINT('Ctrl Pts',(13.2399089726958,0.274038390871736,4.37454348113122));
#21511=CARTESIAN_POINT('Ctrl Pts',(13.2320376006459,0.326885582178656,4.32067233995558));
#21512=CARTESIAN_POINT('Ctrl Pts',(13.2241662285959,0.379732773485576,4.26680119877995));
#21513=CARTESIAN_POINT('Ctrl Pts',(13.2162948565459,0.418980009927931,4.19958860240569));
#21514=CARTESIAN_POINT('Ctrl Pts',(13.208423484496,0.439924354792367,4.12708853413817));
#21515=CARTESIAN_POINT('Ctrl Pts',(13.200552112446,0.460868699656804,4.05458846587065));
#21516=CARTESIAN_POINT('Ctrl Pts',(13.1926807403961,0.463510152943321,3.97680092570987));
#21517=CARTESIAN_POINT('Ctrl Pts',(13.1848093683461,0.447532193317848,3.90304707640827));
#21518=CARTESIAN_POINT('Ctrl Pts',(13.1769379962962,0.431554233692375,3.82929322710668));
#21519=CARTESIAN_POINT('Ctrl Pts',(13.1690666242462,0.396956861154912,3.75957306866428));
#21520=CARTESIAN_POINT('Ctrl Pts',(13.1611952521963,0.347885826291745,3.70224106173923));
#21521=CARTESIAN_POINT('Ctrl Pts',(13.1533238801463,0.298814791428577,3.64490905481418));
#21522=CARTESIAN_POINT('Ctrl Pts',(13.1454525080963,0.235270094239705,3.59996519940648));
#21523=CARTESIAN_POINT('Ctrl Pts',(13.1375811360464,0.164866199243897,3.57279504942506));
#21524=CARTESIAN_POINT('Ctrl Pts',(13.1297097639964,0.0944623042480882,
3.54562489944363));
#21525=CARTESIAN_POINT('Ctrl Pts',(13.1218383919465,0.0171992114453437,
3.53622845488849));
#21526=CARTESIAN_POINT('Ctrl Pts',(13.1139670198965,-0.0576647601420857,
3.54573167743434));
#21527=CARTESIAN_POINT('Ctrl Pts',(13.1060956478466,-0.132528731729515,
3.55523489998019));
#21528=CARTESIAN_POINT('Ctrl Pts',(13.0982242757966,-0.204993582101629,
3.58363778962703));
#21529=CARTESIAN_POINT('Ctrl Pts',(13.0903529037467,-0.266375958336211,
3.62753687126191));
#21530=CARTESIAN_POINT('Ctrl Pts',(13.0824815316967,-0.327758334570793,
3.67143595289679));
#21531=CARTESIAN_POINT('Ctrl Pts',(13.0746101596467,-0.378058236667844,
3.73083122651971));
#21532=CARTESIAN_POINT('Ctrl Pts',(13.0667387875968,-0.411248303781717,
3.79860544673343));
#21533=CARTESIAN_POINT('Ctrl Pts',(13.0588674155468,-0.444438370895591,
3.86637966694714));
#21534=CARTESIAN_POINT('Ctrl Pts',(13.0509960434969,-0.460518603026287,
3.94253283375165));
#21535=CARTESIAN_POINT('Ctrl Pts',(13.0431246714469,-0.457562130387816,
4.0179396288708));
#21536=CARTESIAN_POINT('Ctrl Pts',(13.035253299397,-0.454605657749345,4.09334642398995));
#21537=CARTESIAN_POINT('Ctrl Pts',(13.027381927347,-0.432612480341706,4.16800684742375));
#21538=CARTESIAN_POINT('Ctrl Pts',(13.0195105552971,-0.394218007200806,
4.23297445406563));
#21539=CARTESIAN_POINT('Ctrl Pts',(13.0116391832471,-0.355823534059905,
4.29794206070751));
#21540=CARTESIAN_POINT('Ctrl Pts',(13.0037678111972,-0.301027765185743,
4.35321685055749));
#21541=CARTESIAN_POINT('Ctrl Pts',(12.9958964391472,-0.236396794305188,
4.39217532952931));
#21542=CARTESIAN_POINT('Ctrl Pts',(12.9880250670972,-0.171765823424632,
4.43113380850113));
#21543=CARTESIAN_POINT('Ctrl Pts',(12.9801536950473,-0.0972996505376846,
4.45377597659478));
#21544=CARTESIAN_POINT('Ctrl Pts',(12.9722823229973,-0.0219214440120968,
4.4573886572069));
#21545=CARTESIAN_POINT('Ctrl Pts',(12.9715201181599,-0.014622381881285,
4.45773848219561));
#21546=CARTESIAN_POINT('Ctrl Pts',(12.9707579133226,-0.00731476803234869,
4.45790987647069));
#21547=CARTESIAN_POINT('Ctrl Pts',(12.9699957084852,-6.90274666573233E-6,
4.45790451736119));
#21548=CARTESIAN_POINT('Ctrl Pts',(13.0800042915148,2.8196954984682E-6,
4.45783894202495));
#21549=CARTESIAN_POINT('Ctrl Pts',(13.084269570097,-0.0409086678841046,
4.4578299978409));
#21550=CARTESIAN_POINT('Ctrl Pts',(13.0885348486792,-0.0818224858219862,
4.45239605085009));
#21551=CARTESIAN_POINT('Ctrl Pts',(13.0928001272613,-0.121255029803553,
4.44156782927524));
#21552=CARTESIAN_POINT('Ctrl Pts',(13.1006714993113,-0.194025944662995,
4.42158485301405));
#21553=CARTESIAN_POINT('Ctrl Pts',(13.1085428713613,-0.261752088439453,
4.3832306090213));
#21554=CARTESIAN_POINT('Ctrl Pts',(13.1164142434112,-0.31631794022257,4.33110102808186));
#21555=CARTESIAN_POINT('Ctrl Pts',(13.1242856154612,-0.370883792005687,
4.27897144714243));
#21556=CARTESIAN_POINT('Ctrl Pts',(13.1321569875111,-0.412289351795463,
4.21306652925631));
#21557=CARTESIAN_POINT('Ctrl Pts',(13.1400283595611,-0.435573054271055,
4.14128356060242));
#21558=CARTESIAN_POINT('Ctrl Pts',(13.147899731611,-0.458856756746647,4.06950059194853));
#21559=CARTESIAN_POINT('Ctrl Pts',(13.155771103661,-0.464018601908056,3.99183957252686));
#21560=CARTESIAN_POINT('Ctrl Pts',(13.1636424757109,-0.45044005369213,3.91760650430194));
#21561=CARTESIAN_POINT('Ctrl Pts',(13.1715138477609,-0.436861505476204,
3.84337343607703));
#21562=CARTESIAN_POINT('Ctrl Pts',(13.1793852198109,-0.404542563882944,
3.77256831904885));
#21563=CARTESIAN_POINT('Ctrl Pts',(13.1872565918608,-0.357355958580309,
3.7136756228145));
#21564=CARTESIAN_POINT('Ctrl Pts',(13.1951279639108,-0.310169353277673,
3.65478292658016));
#21565=CARTESIAN_POINT('Ctrl Pts',(13.2029993359607,-0.248115084265664,
3.60780265113964));
#21566=CARTESIAN_POINT('Ctrl Pts',(13.2108707080107,-0.178629020319019,
3.57836437152041));
#21567=CARTESIAN_POINT('Ctrl Pts',(13.2187420800606,-0.109142956372374,
3.54892609190117));
#21568=CARTESIAN_POINT('Ctrl Pts',(13.2266134521106,-0.0322250974910928,
3.53702980810322));
#21569=CARTESIAN_POINT('Ctrl Pts',(13.2344848241605,0.0429076061587562,
3.54410103373967));
#21570=CARTESIAN_POINT('Ctrl Pts',(13.2423561962105,0.118040309808605,3.55117225937612));
#21571=CARTESIAN_POINT('Ctrl Pts',(13.2502275682605,0.191387858227023,3.57721099444696));
#21572=CARTESIAN_POINT('Ctrl Pts',(13.2580989403104,0.254161126126225,3.61909705689013));
#21573=CARTESIAN_POINT('Ctrl Pts',(13.2659703123604,0.316934394025428,3.66098311933329));
#21574=CARTESIAN_POINT('Ctrl Pts',(13.2738416844103,0.369133381405416,3.71871650914877));
#21575=CARTESIAN_POINT('Ctrl Pts',(13.2817130564603,0.404503162915977,3.78537912195109));
#21576=CARTESIAN_POINT('Ctrl Pts',(13.2895844285102,0.43987294442654,3.85204173475342));
#21577=CARTESIAN_POINT('Ctrl Pts',(13.2974558005602,0.458413520067676,3.92763357054259));
#21578=CARTESIAN_POINT('Ctrl Pts',(13.3053271726101,0.457903200829578,4.00309657448501));
#21579=CARTESIAN_POINT('Ctrl Pts',(13.3131985446601,0.457392881591479,4.07855957842742));
#21580=CARTESIAN_POINT('Ctrl Pts',(13.3210699167101,0.437831667474148,4.15389375052308));
#21581=CARTESIAN_POINT('Ctrl Pts',(13.32894128876,0.401563549045306,4.22007191138728));
#21582=CARTESIAN_POINT('Ctrl Pts',(13.33681266081,0.365295430616463,4.28625007225149));
#21583=CARTESIAN_POINT('Ctrl Pts',(13.3446840328599,0.31232040787611,4.34327222188425));
#21584=CARTESIAN_POINT('Ctrl Pts',(13.3525554049099,0.248986397312635,4.38430548273058));
#21585=CARTESIAN_POINT('Ctrl Pts',(13.3604267769598,0.185652386749161,4.42533874357692));
#21586=CARTESIAN_POINT('Ctrl Pts',(13.3682981490098,0.111959388362564,4.45038311563682));
#21587=CARTESIAN_POINT('Ctrl Pts',(13.3761695210597,0.0367379221854645,
4.45643756985705));
#21588=CARTESIAN_POINT('Ctrl Pts',(13.3774477778781,0.024522472144774,4.45742077168506));
#21589=CARTESIAN_POINT('Ctrl Pts',(13.3787260346965,0.0122667140672706,
4.45790318029249));
#21590=CARTESIAN_POINT('Ctrl Pts',(13.3800042915148,1.00338821889499E-5,
4.45789143379912));
#21591=CARTESIAN_POINT('Origin',(12.5,0.,4.));
#21592=CARTESIAN_POINT('',(13.6800042915148,-8.85210990424201E-6,4.45789764648838));
#21593=CARTESIAN_POINT('',(13.5699957084852,1.03170790782398E-5,4.4578580083501));
#21594=CARTESIAN_POINT('',(12.5,-5.60735153159594E-17,4.457875));
#21595=CARTESIAN_POINT('Ctrl Pts',(13.5699957084852,1.03170790782398E-5,
4.4578580083501));
#21596=CARTESIAN_POINT('Ctrl Pts',(13.5675422145714,0.0235408097699949,
4.45787795556699));
#21597=CARTESIAN_POINT('Ctrl Pts',(13.5650887206577,0.0470683081483061,
4.45609516914004));
#21598=CARTESIAN_POINT('Ctrl Pts',(13.562635226744,0.0703115975725277,4.45248338388903));
#21599=CARTESIAN_POINT('Ctrl Pts',(13.554763854694,0.144881409096958,4.44089594716616));
#21600=CARTESIAN_POINT('Ctrl Pts',(13.5468924826441,0.21652593236894,4.41048310506186));
#21601=CARTESIAN_POINT('Ctrl Pts',(13.5390211105941,0.276660113016528,4.36488918223832));
#21602=CARTESIAN_POINT('Ctrl Pts',(13.5311497385442,0.336794293664116,4.31929525941478));
#21603=CARTESIAN_POINT('Ctrl Pts',(13.5232783664942,0.385418131687311,4.25852025587201));
#21604=CARTESIAN_POINT('Ctrl Pts',(13.5154069944443,0.416705106451492,4.18984674794718));
#21605=CARTESIAN_POINT('Ctrl Pts',(13.5075356223943,0.447992081215673,4.12117324002235));
#21606=CARTESIAN_POINT('Ctrl Pts',(13.4996642503443,0.461942192720839,4.04460122771548));
#21607=CARTESIAN_POINT('Ctrl Pts',(13.4917928782944,0.456883820300162,3.96930621892307));
#21608=CARTESIAN_POINT('Ctrl Pts',(13.4839215062444,0.451825447879485,3.89401121013066));
#21609=CARTESIAN_POINT('Ctrl Pts',(13.4760501341945,0.427758591532965,3.81999320485271));
#21610=CARTESIAN_POINT('Ctrl Pts',(13.4681787621445,0.387567146091087,3.75612166820384));
#21611=CARTESIAN_POINT('Ctrl Pts',(13.4603073900946,0.347375700649209,3.69225013155497));
#21612=CARTESIAN_POINT('Ctrl Pts',(13.4524360180446,0.291059666111973,3.63852506353517));
#21613=CARTESIAN_POINT('Ctrl Pts',(13.4445646459947,0.225367307335285,3.60138425741911));
#21614=CARTESIAN_POINT('Ctrl Pts',(13.4366932739447,0.159674948558598,3.56424345130305));
#21615=CARTESIAN_POINT('Ctrl Pts',(13.4288219018947,0.0846062655424597,
3.54368690709073));
#21616=CARTESIAN_POINT('Ctrl Pts',(13.4209505298448,0.00915662451852634,
3.54217788424291));
#21617=CARTESIAN_POINT('Ctrl Pts',(13.4130791577948,-0.0662930165054059,
3.54066886139509));
#21618=CARTESIAN_POINT('Ctrl Pts',(13.4052077857449,-0.142123615537132,
3.55820735991178));
#21619=CARTESIAN_POINT('Ctrl Pts',(13.3973364136949,-0.209248507106454,
3.5926917681625));
#21620=CARTESIAN_POINT('Ctrl Pts',(13.389465041645,-0.276373398675776,3.62717617641322));
#21621=CARTESIAN_POINT('Ctrl Pts',(13.381593669595,-0.334792582782693,3.67860649439798));
#21622=CARTESIAN_POINT('Ctrl Pts',(13.3737222975451,-0.377505777353741,
3.74081990525232));
#21623=CARTESIAN_POINT('Ctrl Pts',(13.3658509254951,-0.420218971924789,
3.80303331610666));
#21624=CARTESIAN_POINT('Ctrl Pts',(13.3579795534451,-0.44722617695997,3.87602981983059));
#21625=CARTESIAN_POINT('Ctrl Pts',(13.3501081813952,-0.455291160112798,
3.95106235628872));
#21626=CARTESIAN_POINT('Ctrl Pts',(13.3422368093452,-0.463356143265626,
4.02609489274685));
#21627=CARTESIAN_POINT('Ctrl Pts',(13.3343654372953,-0.452478904536101,
4.10316346193917));
#21628=CARTESIAN_POINT('Ctrl Pts',(13.3264940652453,-0.423962846915058,
4.17303305431203));
#21629=CARTESIAN_POINT('Ctrl Pts',(13.3186226931954,-0.395446789294015,
4.24290264668488));
#21630=CARTESIAN_POINT('Ctrl Pts',(13.3107513211454,-0.349291912781453,
4.30557326223827));
#21631=CARTESIAN_POINT('Ctrl Pts',(13.3028799490955,-0.291028886105345,
4.35353517632783));
#21632=CARTESIAN_POINT('Ctrl Pts',(13.2950085770455,-0.232765859429236,
4.4014970904174));
#21633=CARTESIAN_POINT('Ctrl Pts',(13.2871372049956,-0.162394682589579,
4.43475030304313));
#21634=CARTESIAN_POINT('Ctrl Pts',(13.2792658329456,-0.0883478267899694,
4.44931013225873));
#21635=CARTESIAN_POINT('Ctrl Pts',(13.2761757914588,-0.059279469337623,
4.4550258417985));
#21636=CARTESIAN_POINT('Ctrl Pts',(13.273085749972,-0.0296446570187532,
4.45786073445524));
#21637=CARTESIAN_POINT('Ctrl Pts',(13.2699957084852,-6.83105689078257E-6,
4.45784477598907));
#21638=CARTESIAN_POINT('Ctrl Pts',(13.3800042915148,1.00338821889499E-5,
4.45789143379912));
#21639=CARTESIAN_POINT('Ctrl Pts',(13.3865974067464,-0.0632086430349686,
4.45783084661254));
#21640=CARTESIAN_POINT('Ctrl Pts',(13.393190521978,-0.12645185159805,4.44462381290384));
#21641=CARTESIAN_POINT('Ctrl Pts',(13.3997836372096,-0.184315051738561,
4.41918121595096));
#21642=CARTESIAN_POINT('Ctrl Pts',(13.4076550092596,-0.253396625517876,
4.3888058714441));
#21643=CARTESIAN_POINT('Ctrl Pts',(13.4155263813095,-0.314809839108902,
4.34099064604983));
#21644=CARTESIAN_POINT('Ctrl Pts',(13.4233977533595,-0.361195640434018,
4.28146516557999));
#21645=CARTESIAN_POINT('Ctrl Pts',(13.4312691254094,-0.407581441759134,
4.22193968511016));
#21646=CARTESIAN_POINT('Ctrl Pts',(13.4391404974594,-0.438939830818339,
4.15070394956476));
#21647=CARTESIAN_POINT('Ctrl Pts',(13.4470118695093,-0.451513179494438,
4.07629402890356));
#21648=CARTESIAN_POINT('Ctrl Pts',(13.4548832415593,-0.464086528170537,
4.00188410824235));
#21649=CARTESIAN_POINT('Ctrl Pts',(13.4627546136093,-0.457874836463529,
3.92430000246534));
#21650=CARTESIAN_POINT('Ctrl Pts',(13.4706259856592,-0.433622441953051,
3.85283849709185));
#21651=CARTESIAN_POINT('Ctrl Pts',(13.4784973577092,-0.409370047442573,
3.78137699171835));
#21652=CARTESIAN_POINT('Ctrl Pts',(13.4863687297591,-0.367076950128625,
3.71603808674838));
#21653=CARTESIAN_POINT('Ctrl Pts',(13.4942401018091,-0.311811067605128,
3.66465124389307));
#21654=CARTESIAN_POINT('Ctrl Pts',(13.502111473859,-0.25654518508163,3.61326440103776));
#21655=CARTESIAN_POINT('Ctrl Pts',(13.509982845909,-0.188306517348584,3.5758296202971));
#21656=CARTESIAN_POINT('Ctrl Pts',(13.5178542179589,-0.115272000283325,
3.55683265457144));
#21657=CARTESIAN_POINT('Ctrl Pts',(13.5257255900089,-0.0422374832180674,
3.53783568884578));
#21658=CARTESIAN_POINT('Ctrl Pts',(13.5335969620589,0.035592883179403,3.53727653813511));
#21659=CARTESIAN_POINT('Ctrl Pts',(13.5414683341088,0.108892804353757,3.55522220461956));
#21660=CARTESIAN_POINT('Ctrl Pts',(13.5493397061588,0.182192725528112,3.573167871104));
#21661=CARTESIAN_POINT('Ctrl Pts',(13.5572110782087,0.250962201479351,3.60961835478357));
#21662=CARTESIAN_POINT('Ctrl Pts',(13.5650824502587,0.306960690387823,3.66020584957927));
#21663=CARTESIAN_POINT('Ctrl Pts',(13.5729538223086,0.362959179296295,3.71079334437498));
#21664=CARTESIAN_POINT('Ctrl Pts',(13.5808251943586,0.406186681162,3.77551785028682));
#21665=CARTESIAN_POINT('Ctrl Pts',(13.5886965664085,0.431463310113251,3.84662352810933));
#21666=CARTESIAN_POINT('Ctrl Pts',(13.5965679384585,0.456739939064502,3.91772920593184));
#21667=CARTESIAN_POINT('Ctrl Pts',(13.6044393105085,0.464065695101298,3.99521605566501));
#21668=CARTESIAN_POINT('Ctrl Pts',(13.6123106825584,0.452562744007997,4.06979894583348));
#21669=CARTESIAN_POINT('Ctrl Pts',(13.6201820546084,0.441059792914696,4.14438183600196));
#21670=CARTESIAN_POINT('Ctrl Pts',(13.6280534266583,0.410728134691299,4.21606076660573));
#21671=CARTESIAN_POINT('Ctrl Pts',(13.6359247987083,0.365202365858889,4.27624656029457));
#21672=CARTESIAN_POINT('Ctrl Pts',(13.6437961707582,0.319676597026479,4.33643235398341));
#21673=CARTESIAN_POINT('Ctrl Pts',(13.6516675428082,0.258956717585058,4.38512501075732));
#21674=CARTESIAN_POINT('Ctrl Pts',(13.6595389148581,0.190318698434502,4.41648976353532));
#21675=CARTESIAN_POINT('Ctrl Pts',(13.666360707077,0.130832969391341,4.44367229602021));
#21676=CARTESIAN_POINT('Ctrl Pts',(13.6731824992959,0.065399948454096,4.45783988979956));
#21677=CARTESIAN_POINT('Ctrl Pts',(13.6800042915148,-8.85210990424201E-6,
4.45789764648838));
#21678=CARTESIAN_POINT('Origin',(12.5,0.,4.));
#21679=CARTESIAN_POINT('',(13.9800042915148,-4.68615130337092E-6,4.45784092071359));
#21680=CARTESIAN_POINT('',(13.8699957084852,1.23414887176878E-6,4.4579133809027));
#21681=CARTESIAN_POINT('',(12.5,-5.60735153159594E-17,4.457875));
#21682=CARTESIAN_POINT('Ctrl Pts',(13.8699957084852,1.23414887176878E-6,
4.4579133809027));
#21683=CARTESIAN_POINT('Ctrl Pts',(13.8698700512209,0.00120594270822336,
4.45791357044259));
#21684=CARTESIAN_POINT('Ctrl Pts',(13.8697443939566,0.00241064979645091,
4.45790891401425));
#21685=CARTESIAN_POINT('Ctrl Pts',(13.8696187366923,0.00361531855258033,
4.45789940262096));
#21686=CARTESIAN_POINT('Ctrl Pts',(13.8617473646423,0.0790776965455978,
4.45730359373015));
#21687=CARTESIAN_POINT('Ctrl Pts',(13.8538759925924,0.154389660535011,4.43765704798318));
#21688=CARTESIAN_POINT('Ctrl Pts',(13.8460046205424,0.22052669229976,4.40131398110731));
#21689=CARTESIAN_POINT('Ctrl Pts',(13.8381332484924,0.286663724064511,4.36497091423144));
#21690=CARTESIAN_POINT('Ctrl Pts',(13.8302618764425,0.343625823604597,4.31193132622667));
#21691=CARTESIAN_POINT('Ctrl Pts',(13.8223905043925,0.384587309076409,4.24855087033892));
#21692=CARTESIAN_POINT('Ctrl Pts',(13.8145191323426,0.42554879454822,4.18517041445118));
#21693=CARTESIAN_POINT('Ctrl Pts',(13.8066477602926,0.450509665951756,4.11144909068046));
#21694=CARTESIAN_POINT('Ctrl Pts',(13.7987763882427,0.456478899990553,4.03622081324714));
#21695=CARTESIAN_POINT('Ctrl Pts',(13.7909050161927,0.46244813402935,3.96099253581381));
#21696=CARTESIAN_POINT('Ctrl Pts',(13.7830336441427,0.449425730703409,3.88425730471787));
#21697=CARTESIAN_POINT('Ctrl Pts',(13.7751622720928,0.418972144817937,3.81521018611534));
#21698=CARTESIAN_POINT('Ctrl Pts',(13.7672909000428,0.388518558932466,3.74616306751281));
#21699=CARTESIAN_POINT('Ctrl Pts',(13.7594195279929,0.340633790487464,3.68480406140369));
#21700=CARTESIAN_POINT('Ctrl Pts',(13.7515481559429,0.281055798532888,3.6384857242654));
#21701=CARTESIAN_POINT('Ctrl Pts',(13.743676783893,0.221477806578313,3.59216738712712));
#21702=CARTESIAN_POINT('Ctrl Pts',(13.735805411843,0.150206591114165,3.56088971895966));
#21703=CARTESIAN_POINT('Ctrl Pts',(13.7279340397931,0.0757824736049535,
3.54840067521841));
#21704=CARTESIAN_POINT('Ctrl Pts',(13.7200626677431,0.00135835609574232,
3.53591163147717));
#21705=CARTESIAN_POINT('Ctrl Pts',(13.7121912956931,-0.0762186634585312,
3.54221121216214));
#21706=CARTESIAN_POINT('Ctrl Pts',(13.7043199236432,-0.14765264866984,3.56654454809098));
#21707=CARTESIAN_POINT('Ctrl Pts',(13.6964485515932,-0.219086633881149,
3.59087788401983));
#21708=CARTESIAN_POINT('Ctrl Pts',(13.6885771795433,-0.284377584749494,
3.63324497519255));
#21709=CARTESIAN_POINT('Ctrl Pts',(13.6807058074933,-0.335701785830877,
3.68856903744356));
#21710=CARTESIAN_POINT('Ctrl Pts',(13.6728344354434,-0.38702598691226,3.74389309969457));
#21711=CARTESIAN_POINT('Ctrl Pts',(13.6649630633934,-0.424383438206683,
3.81217413302386));
#21712=CARTESIAN_POINT('Ctrl Pts',(13.6570916913435,-0.443297653083863,
3.88523012494906));
#21713=CARTESIAN_POINT('Ctrl Pts',(13.6492203192935,-0.462211867961044,
3.95828611687427));
#21714=CARTESIAN_POINT('Ctrl Pts',(13.6413489472436,-0.462682846420982,
4.03611706739538));
#21715=CARTESIAN_POINT('Ctrl Pts',(13.6334775751936,-0.444654151830396,
4.10939661196244));
#21716=CARTESIAN_POINT('Ctrl Pts',(13.6256062031436,-0.42662545723981,4.18267615652949));
#21717=CARTESIAN_POINT('Ctrl Pts',(13.6177348310937,-0.3900970895987,4.25140429514248));
#21718=CARTESIAN_POINT('Ctrl Pts',(13.6098634590437,-0.339446187702822,
4.3073454393722));
#21719=CARTESIAN_POINT('Ctrl Pts',(13.6019920869938,-0.288795285806945,
4.36328658360191));
#21720=CARTESIAN_POINT('Ctrl Pts',(13.5941207149438,-0.224021849656302,
4.40644073344835));
#21721=CARTESIAN_POINT('Ctrl Pts',(13.5862493428939,-0.152887581692542,
4.43163679270085));
#21722=CARTESIAN_POINT('Ctrl Pts',(13.5808314647576,-0.103925749791867,
4.44897928111035));
#21723=CARTESIAN_POINT('Ctrl Pts',(13.5754135866214,-0.0519504158054226,
4.45781396031326));
#21724=CARTESIAN_POINT('Ctrl Pts',(13.5699957084852,1.03170790782398E-5,
4.4578580083501));
#21725=CARTESIAN_POINT('Ctrl Pts',(13.6800042915148,-8.85210990424201E-6,
4.45789764648838));
#21726=CARTESIAN_POINT('Ctrl Pts',(13.6810538713459,-0.010072447664127,
4.45790653275371));
#21727=CARTESIAN_POINT('Ctrl Pts',(13.6821034511769,-0.0201354698749596,
4.45758141170421));
#21728=CARTESIAN_POINT('Ctrl Pts',(13.683153031008,-0.0301761699425476,
4.45691829561871));
#21729=CARTESIAN_POINT('Ctrl Pts',(13.691024403058,-0.105476860309351,4.45194522614199));
#21730=CARTESIAN_POINT('Ctrl Pts',(13.6988957751079,-0.179522082183268,
4.42796223840642));
#21731=CARTESIAN_POINT('Ctrl Pts',(13.7067671471579,-0.24343910912634,4.38784317739428));
#21732=CARTESIAN_POINT('Ctrl Pts',(13.7146385192078,-0.307356136069411,
4.34772411638213));
#21733=CARTESIAN_POINT('Ctrl Pts',(13.7225098912578,-0.361144968081636,
4.2914689820934));
#21734=CARTESIAN_POINT('Ctrl Pts',(13.7303812633077,-0.398360171146024,
4.22581874179975));
#21735=CARTESIAN_POINT('Ctrl Pts',(13.7382526353577,-0.435575374210412,
4.1601685015061));
#21736=CARTESIAN_POINT('Ctrl Pts',(13.7461240074077,-0.456216948326962,
4.08512315520753));
#21737=CARTESIAN_POINT('Ctrl Pts',(13.7539953794576,-0.457811445030669,
4.00967527273228));
#21738=CARTESIAN_POINT('Ctrl Pts',(13.7618667515076,-0.459405941734377,
3.93422739025703));
#21739=CARTESIAN_POINT('Ctrl Pts',(13.7697381235575,-0.441953361025241,
3.85837697160509));
#21740=CARTESIAN_POINT('Ctrl Pts',(13.7776094956075,-0.407545019133394,
3.79121305720166));
#21741=CARTESIAN_POINT('Ctrl Pts',(13.7854808676574,-0.373136677241547,
3.72404914279823));
#21742=CARTESIAN_POINT('Ctrl Pts',(13.7933522397074,-0.321772574166988,
3.6655717326433));
#21743=CARTESIAN_POINT('Ctrl Pts',(13.8012236117573,-0.259607592342073,
3.6227880859492));
#21744=CARTESIAN_POINT('Ctrl Pts',(13.8090949838073,-0.19744261051716,3.5800044392551));
#21745=CARTESIAN_POINT('Ctrl Pts',(13.8169663558573,-0.124476749941891,
3.55291455602183));
#21746=CARTESIAN_POINT('Ctrl Pts',(13.8248377279072,-0.0494533988297167,
3.54476457579874));
#21747=CARTESIAN_POINT('Ctrl Pts',(13.8327090999572,0.0255699522824598,
3.53661459557564));
#21748=CARTESIAN_POINT('Ctrl Pts',(13.8405804720071,0.102650793931542,3.54740451836272));
#21749=CARTESIAN_POINT('Ctrl Pts',(13.8484518440571,0.172552645974024,3.57584140410587));
#21750=CARTESIAN_POINT('Ctrl Pts',(13.856323216107,0.242454498016503,3.60427828984902));
#21751=CARTESIAN_POINT('Ctrl Pts',(13.864194588157,0.305177360452382,3.65036213854823));
#21752=CARTESIAN_POINT('Ctrl Pts',(13.8720659602069,0.353205247972751,3.70857079263049));
#21753=CARTESIAN_POINT('Ctrl Pts',(13.8799373322569,0.40123313549312,3.76677944671275));
#21754=CARTESIAN_POINT('Ctrl Pts',(13.8878087043068,0.434566048097978,3.83711290617806));
#21755=CARTESIAN_POINT('Ctrl Pts',(13.8956800763568,0.44920975351361,3.9111432194385));
#21756=CARTESIAN_POINT('Ctrl Pts',(13.9035514484068,0.463853458929242,3.98517353269893));
#21757=CARTESIAN_POINT('Ctrl Pts',(13.9114228204567,0.459807957155645,4.06290069975448));
#21758=CARTESIAN_POINT('Ctrl Pts',(13.9192941925067,0.437558014523894,4.13501079227018));
#21759=CARTESIAN_POINT('Ctrl Pts',(13.9271655645566,0.415308071892144,4.20712088478587));
#21760=CARTESIAN_POINT('Ctrl Pts',(13.9350369366066,0.374853688402242,4.27361390276169));
#21761=CARTESIAN_POINT('Ctrl Pts',(13.9429083086565,0.321042451364188,4.32652208887851));
#21762=CARTESIAN_POINT('Ctrl Pts',(13.9507796807065,0.267231214326134,4.37943027499533));
#21763=CARTESIAN_POINT('Ctrl Pts',(13.9586510527564,0.200063123739928,4.41875362925314));
#21764=CARTESIAN_POINT('Ctrl Pts',(13.9665224248064,0.127586829849962,4.43978009385641));
#21765=CARTESIAN_POINT('Ctrl Pts',(13.9710163803759,0.086208370984788,4.45178460807712));
#21766=CARTESIAN_POINT('Ctrl Pts',(13.9755103359454,0.0430996806131821,
4.45782517307841));
#21767=CARTESIAN_POINT('Ctrl Pts',(13.9800042915148,-4.68615130337092E-6,
4.45784092071359));
#21768=CARTESIAN_POINT('Origin',(12.5,0.,4.));
#21769=CARTESIAN_POINT('',(14.2800042915148,1.11332528513013E-5,4.45786561359635));
#21770=CARTESIAN_POINT('',(14.1699957084852,-1.10604184835328E-5,4.4578646218584));
#21771=CARTESIAN_POINT('',(12.5,-5.60735153159594E-17,4.457875));
#21772=CARTESIAN_POINT('Ctrl Pts',(14.1699957084852,-1.10604184835328E-5,
4.4578646218584));
#21773=CARTESIAN_POINT('Ctrl Pts',(14.1643265158203,0.0543576752587709,
4.45781404039958));
#21774=CARTESIAN_POINT('Ctrl Pts',(14.1586573231555,0.108743966382031,4.44812254260427));
#21775=CARTESIAN_POINT('Ctrl Pts',(14.1529881304907,0.159684023833442,4.42916890146099));
#21776=CARTESIAN_POINT('Ctrl Pts',(14.1451167584407,0.230411580321883,4.40285278028461));
#21777=CARTESIAN_POINT('Ctrl Pts',(14.1372453863907,0.294495541512382,4.358681244225));
#21778=CARTESIAN_POINT('Ctrl Pts',(14.1293740143408,0.344256823700223,4.30194730133701));
#21779=CARTESIAN_POINT('Ctrl Pts',(14.1215026422908,0.394018105888063,4.24521335844902));
#21780=CARTESIAN_POINT('Ctrl Pts',(14.1136312702409,0.429456709073245,4.17591700873265));
#21781=CARTESIAN_POINT('Ctrl Pts',(14.1057598981909,0.446326079279053,4.10236192849032));
#21782=CARTESIAN_POINT('Ctrl Pts',(14.097888526141,0.46319544948486,4.02880684824799));
#21783=CARTESIAN_POINT('Ctrl Pts',(14.090017154091,0.461495586711293,3.95099303747972));
#21784=CARTESIAN_POINT('Ctrl Pts',(14.0821457820411,0.441430182931853,3.87824480690492));
#21785=CARTESIAN_POINT('Ctrl Pts',(14.0742744099911,0.421364779152413,3.80549657633012));
#21786=CARTESIAN_POINT('Ctrl Pts',(14.0664030379411,0.3829338343671,3.73781392594881));
#21787=CARTESIAN_POINT('Ctrl Pts',(14.0585316658912,0.330742470300218,3.68330716492384));
#21788=CARTESIAN_POINT('Ctrl Pts',(14.0506602938412,0.278551106233337,3.62880040389886));
#21789=CARTESIAN_POINT('Ctrl Pts',(14.0427889217913,0.212599322884887,3.58746953223022));
#21790=CARTESIAN_POINT('Ctrl Pts',(14.0349175497413,0.140790022250932,3.5642671654747));
#21791=CARTESIAN_POINT('Ctrl Pts',(14.0270461776914,0.0689807216169763,
3.54106479871918));
#21792=CARTESIAN_POINT('Ctrl Pts',(14.0191748056414,-0.00868609630248519,
3.53599093687678));
#21793=CARTESIAN_POINT('Ctrl Pts',(14.0113034335915,-0.0829037347177578,
3.5496535731032));
#21794=CARTESIAN_POINT('Ctrl Pts',(14.0034320615415,-0.15712137313303,3.56331620932962));
#21795=CARTESIAN_POINT('Ctrl Pts',(13.9955606894916,-0.227889832044114,
3.59571534362485));
#21796=CARTESIAN_POINT('Ctrl Pts',(13.9876893174416,-0.286729034540398,
3.64296863695132));
#21797=CARTESIAN_POINT('Ctrl Pts',(13.9798179453916,-0.345568237036683,
3.69022193027778));
#21798=CARTESIAN_POINT('Ctrl Pts',(13.9719465733417,-0.392478183118168,
3.75232938263547));
#21799=CARTESIAN_POINT('Ctrl Pts',(13.9640752012917,-0.421837725217638,
3.82184875237013));
#21800=CARTESIAN_POINT('Ctrl Pts',(13.9562038292418,-0.451197267317109,
3.8913681221048));
#21801=CARTESIAN_POINT('Ctrl Pts',(13.9483324571918,-0.463006405434566,
3.96829940921644));
#21802=CARTESIAN_POINT('Ctrl Pts',(13.9404610851419,-0.455850068491383,
4.04342405445454));
#21803=CARTESIAN_POINT('Ctrl Pts',(13.9325897130919,-0.448693731548199,
4.11854869969265));
#21804=CARTESIAN_POINT('Ctrl Pts',(13.924718341042,-0.422571919544373,4.19186670305722));
#21805=CARTESIAN_POINT('Ctrl Pts',(13.916846968992,-0.38061476952465,4.25459247959939));
#21806=CARTESIAN_POINT('Ctrl Pts',(13.908975596942,-0.338657619504927,4.31731825614156));
#21807=CARTESIAN_POINT('Ctrl Pts',(13.9011042248921,-0.280865131469307,
4.36945180586132));
#21808=CARTESIAN_POINT('Ctrl Pts',(13.8932328528421,-0.214162491453186,
4.40474604470388));
#21809=CARTESIAN_POINT('Ctrl Pts',(13.8854871380565,-0.148524681204106,
4.43947685223224));
#21810=CARTESIAN_POINT('Ctrl Pts',(13.8777414232708,-0.0742589286223064,
4.45790169736071));
#21811=CARTESIAN_POINT('Ctrl Pts',(13.8699957084852,1.23414887176878E-6,
4.4579133809027));
#21812=CARTESIAN_POINT('Ctrl Pts',(13.9800042915148,-4.68615130337092E-6,
4.45784092071359));
#21813=CARTESIAN_POINT('Ctrl Pts',(13.9833817079953,-0.0323996211791616,
4.45785275579335));
#21814=CARTESIAN_POINT('Ctrl Pts',(13.9867591244758,-0.064792114138131,
4.45446164082457));
#21815=CARTESIAN_POINT('Ctrl Pts',(13.9901365409563,-0.0964458636128916,
4.44764173788363));
#21816=CARTESIAN_POINT('Ctrl Pts',(13.9980079130062,-0.170217765992045,
4.43174734235885));
#21817=CARTESIAN_POINT('Ctrl Pts',(14.0058792850562,-0.239977073556624,
4.39722897636055));
#21818=CARTESIAN_POINT('Ctrl Pts',(14.0137506571061,-0.297364634468633,
4.34822292324149));
#21819=CARTESIAN_POINT('Ctrl Pts',(14.0216220291561,-0.354752195380644,
4.29921687012243));
#21820=CARTESIAN_POINT('Ctrl Pts',(14.0294934012061,-0.399768009640084,
4.23572312988262));
#21821=CARTESIAN_POINT('Ctrl Pts',(14.037364773256,-0.427017900618165,4.16535006094698));
#21822=CARTESIAN_POINT('Ctrl Pts',(14.045236145306,-0.454267791596245,4.09497699201134));
#21823=CARTESIAN_POINT('Ctrl Pts',(14.0531075173559,-0.463751759292965,
4.01772459437987));
#21824=CARTESIAN_POINT('Ctrl Pts',(14.0609788894059,-0.45433335426851,3.94284990548881));
#21825=CARTESIAN_POINT('Ctrl Pts',(14.0688502614558,-0.444914949244056,
3.86797521659775));
#21826=CARTESIAN_POINT('Ctrl Pts',(14.0767216335058,-0.416594171498428,
3.7954782364471));
#21827=CARTESIAN_POINT('Ctrl Pts',(14.0845930055557,-0.372764656800254,
3.7340461680214));
#21828=CARTESIAN_POINT('Ctrl Pts',(14.0924643776057,-0.328935142102078,
3.67261409959569));
#21829=CARTESIAN_POINT('Ctrl Pts',(14.1003357496557,-0.269596890451354,
3.62224694289495));
#21830=CARTESIAN_POINT('Ctrl Pts',(14.1082071217056,-0.201860314388951,
3.58898011778223));
#21831=CARTESIAN_POINT('Ctrl Pts',(14.1160784937556,-0.134123738326549,
3.55571329266952));
#21832=CARTESIAN_POINT('Ctrl Pts',(14.1239498658055,-0.0579888378524715,
3.53954679914483));
#21833=CARTESIAN_POINT('Ctrl Pts',(14.1318212378555,0.0174212575835846,
3.54241784356498));
#21834=CARTESIAN_POINT('Ctrl Pts',(14.1396926099054,0.0928313530196406,
3.54528888798513));
#21835=CARTESIAN_POINT('Ctrl Pts',(14.1475639819554,0.167516643417675,3.56719747035013));
#21836=CARTESIAN_POINT('Ctrl Pts',(14.1554353540053,0.232527703900953,3.60551831852155));
#21837=CARTESIAN_POINT('Ctrl Pts',(14.1633067260553,0.297538764384231,3.64383916669297));
#21838=CARTESIAN_POINT('Ctrl Pts',(14.1711780981053,0.352875594952755,3.69857228067082));
#21839=CARTESIAN_POINT('Ctrl Pts',(14.1790494701552,0.391907267274456,3.76315907456484));
#21840=CARTESIAN_POINT('Ctrl Pts',(14.1869208422052,0.430938939596158,3.82774586845886));
#21841=CARTESIAN_POINT('Ctrl Pts',(14.1947922142551,0.453665453671035,3.90218634226906));
#21842=CARTESIAN_POINT('Ctrl Pts',(14.2026635863051,0.45736352584659,3.97756040711846));
#21843=CARTESIAN_POINT('Ctrl Pts',(14.210534958355,0.461061598022145,4.05293447196787));
#21844=CARTESIAN_POINT('Ctrl Pts',(14.218406330405,0.445731228298378,4.12924212785648));
#21845=CARTESIAN_POINT('Ctrl Pts',(14.2262777024549,0.413209431587385,4.19733954431574));
#21846=CARTESIAN_POINT('Ctrl Pts',(14.2341490745049,0.380687634876391,4.265436960775));
#21847=CARTESIAN_POINT('Ctrl Pts',(14.2420204465549,0.330974411178171,4.32532413780492));
#21848=CARTESIAN_POINT('Ctrl Pts',(14.2498918186048,0.270026820557645,4.36982488597043));
#21849=CARTESIAN_POINT('Ctrl Pts',(14.2577631906548,0.209079229937118,4.41432563413594));
#21850=CARTESIAN_POINT('Ctrl Pts',(14.2656345627047,0.136897272394287,4.44343995343705));
#21851=CARTESIAN_POINT('Ctrl Pts',(14.2735059347547,0.0621304022332317,
4.45367911922619));
#21852=CARTESIAN_POINT('Ctrl Pts',(14.2756720536747,0.0415553447945806,
4.4564968301158));
#21853=CARTESIAN_POINT('Ctrl Pts',(14.2778381725948,0.020784533837212,4.45788513960506));
#21854=CARTESIAN_POINT('Ctrl Pts',(14.2800042915148,1.11332528513013E-5,
4.45786561359635));
#21855=CARTESIAN_POINT('Origin',(12.5,0.,4.));
#21856=CARTESIAN_POINT('',(14.5800042915148,-1.58578451148518E-6,4.45791318879952));
#21857=CARTESIAN_POINT('',(14.4699957084852,4.96934848862042E-6,4.4578413260902));
#21858=CARTESIAN_POINT('',(12.5,-5.60735153159594E-17,4.457875));
#21859=CARTESIAN_POINT('Ctrl Pts',(14.4699957084852,4.96934848862042E-6,
4.4578413260902));
#21860=CARTESIAN_POINT('Ctrl Pts',(14.4666543524698,0.0320539454002899,
4.45785375637851));
#21861=CARTESIAN_POINT('Ctrl Pts',(14.4633129964543,0.0641003838712636,
4.45453523052653));
#21862=CARTESIAN_POINT('Ctrl Pts',(14.4599716404389,0.0954313752779353,
4.44785911407655));
#21863=CARTESIAN_POINT('Ctrl Pts',(14.452100268389,0.169239101517837,4.43213190746217));
#21864=CARTESIAN_POINT('Ctrl Pts',(14.444228896339,0.2390764403586,4.39777168651743));
#21865=CARTESIAN_POINT('Ctrl Pts',(14.4363575242891,0.296574889592956,4.34889578431359));
#21866=CARTESIAN_POINT('Ctrl Pts',(14.4284861522391,0.354073338827311,4.30001988210975));
#21867=CARTESIAN_POINT('Ctrl Pts',(14.4206147801891,0.39923289845526,4.2366282986468));
#21868=CARTESIAN_POINT('Ctrl Pts',(14.4127434081392,0.4266421670589,4.16631715105832));
#21869=CARTESIAN_POINT('Ctrl Pts',(14.4048720360892,0.454051435662541,4.09600600346984));
#21870=CARTESIAN_POINT('Ctrl Pts',(14.3970006640393,0.463710413241873,4.01877529175582));
#21871=CARTESIAN_POINT('Ctrl Pts',(14.3891292919893,0.454461679188747,3.94387945476197));
#21872=CARTESIAN_POINT('Ctrl Pts',(14.3812579199394,0.445212945135621,3.86898361776811));
#21873=CARTESIAN_POINT('Ctrl Pts',(14.3733865478894,0.417056499450037,3.79642265549441));
#21874=CARTESIAN_POINT('Ctrl Pts',(14.3655151758395,0.373366286239542,3.73489143780602));
#21875=CARTESIAN_POINT('Ctrl Pts',(14.3576438037895,0.329676073029047,3.67336022011762));
#21876=CARTESIAN_POINT('Ctrl Pts',(14.3497724317395,0.270452092293641,3.62285874701452));
#21877=CARTESIAN_POINT('Ctrl Pts',(14.3419010596896,0.202791063664024,3.58943853329022));
#21878=CARTESIAN_POINT('Ctrl Pts',(14.3340296876396,0.135130035034407,3.55601831956592));
#21879=CARTESIAN_POINT('Ctrl Pts',(14.3261583155897,0.0590319585105798,
3.53967936522043));
#21880=CARTESIAN_POINT('Ctrl Pts',(14.3182869435397,-0.0163844490157649,
3.54237954232867));
#21881=CARTESIAN_POINT('Ctrl Pts',(14.3104155714898,-0.0918008565421096,
3.54507971943691));
#21882=CARTESIAN_POINT('Ctrl Pts',(14.3025441994398,-0.166535595070972,
3.56681902799889));
#21883=CARTESIAN_POINT('Ctrl Pts',(14.2946728273899,-0.231633314431234,
3.60499247969884));
#21884=CARTESIAN_POINT('Ctrl Pts',(14.2868014553399,-0.296731033791496,
3.64316593139879));
#21885=CARTESIAN_POINT('Ctrl Pts',(14.2789300832899,-0.352191733983158,
3.6977735262367));
#21886=CARTESIAN_POINT('Ctrl Pts',(14.27105871124,-0.391369643565407,3.76227171909014));
#21887=CARTESIAN_POINT('Ctrl Pts',(14.26318733919,-0.430547553147657,3.82676991194359));
#21888=CARTESIAN_POINT('Ctrl Pts',(14.2553159671401,-0.453442672120494,
3.90115870281258));
#21889=CARTESIAN_POINT('Ctrl Pts',(14.2474445950901,-0.457311513162664,
3.97652419590847));
#21890=CARTESIAN_POINT('Ctrl Pts',(14.2395732230402,-0.461180354204834,
4.05188968900435));
#21891=CARTESIAN_POINT('Ctrl Pts',(14.2317018509902,-0.446022917316338,
4.12823188432714));
#21892=CARTESIAN_POINT('Ctrl Pts',(14.2238304789403,-0.413655495130362,
4.19640281260034));
#21893=CARTESIAN_POINT('Ctrl Pts',(14.2159591068903,-0.381288072944386,
4.26457374087354));
#21894=CARTESIAN_POINT('Ctrl Pts',(14.2080877348403,-0.33171066546093,4.32457340209717));
#21895=CARTESIAN_POINT('Ctrl Pts',(14.2002163627904,-0.270864058094251,
4.36921212802613));
#21896=CARTESIAN_POINT('Ctrl Pts',(14.1923449907404,-0.210017450727571,
4.41385085395509));
#21897=CARTESIAN_POINT('Ctrl Pts',(14.1844736186905,-0.137901643477669,
4.44312864458938));
#21898=CARTESIAN_POINT('Ctrl Pts',(14.1766022466405,-0.0631581639595259,
4.45353718675995));
#21899=CARTESIAN_POINT('Ctrl Pts',(14.1744000672554,-0.0422471272657682,
4.45644919204336));
#21900=CARTESIAN_POINT('Ctrl Pts',(14.1721978878703,-0.021130418320356,
4.45788427006097));
#21901=CARTESIAN_POINT('Ctrl Pts',(14.1699957084852,-1.10604184835328E-5,
4.4578646218584));
#21902=CARTESIAN_POINT('Ctrl Pts',(14.2800042915148,1.11332528513013E-5,
4.45786561359635));
#21903=CARTESIAN_POINT('Ctrl Pts',(14.2857095446447,-0.0547030874695854,
4.45781418483069));
#21904=CARTESIAN_POINT('Ctrl Pts',(14.2914147977746,-0.109435272994953,
4.44799629651036));
#21905=CARTESIAN_POINT('Ctrl Pts',(14.2971200509045,-0.16065599949712,4.42880599334559));
#21906=CARTESIAN_POINT('Ctrl Pts',(14.3049914229545,-0.231323748287136,
4.40232968939868));
#21907=CARTESIAN_POINT('Ctrl Pts',(14.3128627950045,-0.295307463087888,
4.35801306922771));
#21908=CARTESIAN_POINT('Ctrl Pts',(14.3207341670544,-0.344940072567234,
4.30116652609615));
#21909=CARTESIAN_POINT('Ctrl Pts',(14.3286055391044,-0.394572682046581,
4.24431998296459));
#21910=CARTESIAN_POINT('Ctrl Pts',(14.3364769111543,-0.429854186204522,
4.17494351687244));
#21911=CARTESIAN_POINT('Ctrl Pts',(14.3443482832043,-0.446556856002091,
4.10135040434572));
#21912=CARTESIAN_POINT('Ctrl Pts',(14.3522196552542,-0.46325952579966,4.027757291819));
#21913=CARTESIAN_POINT('Ctrl Pts',(14.3600910273042,-0.461383361236856,
3.9499475328577));
#21914=CARTESIAN_POINT('Ctrl Pts',(14.3679623993541,-0.441153180262727,
3.87724495265939));
#21915=CARTESIAN_POINT('Ctrl Pts',(14.3758337714041,-0.420922999288597,
3.80454237246108));
#21916=CARTESIAN_POINT('Ctrl Pts',(14.383705143454,-0.382338801903142,3.73694697102576));
#21917=CARTESIAN_POINT('Ctrl Pts',(14.391576515504,-0.330024073856894,3.68255860260764));
#21918=CARTESIAN_POINT('Ctrl Pts',(14.399447887554,-0.277709345810648,3.62817023418952));
#21919=CARTESIAN_POINT('Ctrl Pts',(14.4073192596039,-0.21166408710361,3.58698889878861));
#21920=CARTESIAN_POINT('Ctrl Pts',(14.4151906316539,-0.139802400742051,
3.56394929325792));
#21921=CARTESIAN_POINT('Ctrl Pts',(14.4230620037038,-0.0679407143804897,
3.54090968772722));
#21922=CARTESIAN_POINT('Ctrl Pts',(14.4309333757538,0.00973739963559066,
3.53601181206673));
#21923=CARTESIAN_POINT('Ctrl Pts',(14.4388047478037,0.0839238909224197,
3.54984257127538));
#21924=CARTESIAN_POINT('Ctrl Pts',(14.4466761198537,0.158110382209248,3.56367333048403));
#21925=CARTESIAN_POINT('Ctrl Pts',(14.4545474919037,0.228805250766822,3.59623272456181));
#21926=CARTESIAN_POINT('Ctrl Pts',(14.4624188639536,0.287537237904754,3.64361921078484));
#21927=CARTESIAN_POINT('Ctrl Pts',(14.4702902360036,0.346269225042686,3.69100569700788));
#21928=CARTESIAN_POINT('Ctrl Pts',(14.4781616080535,0.393038330760977,3.75321927537615));
#21929=CARTESIAN_POINT('Ctrl Pts',(14.4860329801035,0.422240284179214,3.8228049873169));
#21930=CARTESIAN_POINT('Ctrl Pts',(14.4939043521534,0.451442237597453,3.89239069925764));
#21931=CARTESIAN_POINT('Ctrl Pts',(14.5017757242034,0.463077038715637,3.96934854477086));
#21932=CARTESIAN_POINT('Ctrl Pts',(14.5096470962533,0.45575050699275,4.04445678215295));
#21933=CARTESIAN_POINT('Ctrl Pts',(14.5175184683033,0.448423975269863,4.11956501953505));
#21934=CARTESIAN_POINT('Ctrl Pts',(14.5253898403532,0.422136110705906,4.19282364878603));
#21935=CARTESIAN_POINT('Ctrl Pts',(14.5332612124032,0.380036948171907,4.2554541996672));
#21936=CARTESIAN_POINT('Ctrl Pts',(14.5411325844532,0.337937785637909,4.31808475054837));
#21937=CARTESIAN_POINT('Ctrl Pts',(14.5490039565031,0.28002732513387,4.37008722305972));
#21938=CARTESIAN_POINT('Ctrl Pts',(14.5568753285531,0.213244889156206,4.40523023992844));
#21939=CARTESIAN_POINT('Ctrl Pts',(14.5645849828737,0.147834501639678,4.43965124177167));
#21940=CARTESIAN_POINT('Ctrl Pts',(14.5722946371942,0.0739129441497101,
4.45789842831743));
#21941=CARTESIAN_POINT('Ctrl Pts',(14.5800042915148,-1.58578451148518E-6,
4.45791318879952));
#21942=CARTESIAN_POINT('Origin',(12.5,0.,4.));
#21943=CARTESIAN_POINT('',(14.8800042915148,-1.01702808208336E-5,4.45785711824254));
#21944=CARTESIAN_POINT('',(14.7699957084852,8.6346448269735E-6,4.45789857801605));
#21945=CARTESIAN_POINT('',(12.5,-5.60735153159594E-17,4.457875));
#21946=CARTESIAN_POINT('Ctrl Pts',(14.7699957084852,8.6346448269735E-6,
4.45789857801605));
#21947=CARTESIAN_POINT('Ctrl Pts',(14.7689821891192,0.00972641784825355,
4.45790700998655));
#21948=CARTESIAN_POINT('Ctrl Pts',(14.7679686697532,0.01944367562558,4.45760386164098));
#21949=CARTESIAN_POINT('Ctrl Pts',(14.7669551503872,0.0291408329004781,
4.45698549795522));
#21950=CARTESIAN_POINT('Ctrl Pts',(14.7590837783372,0.104452598317788,4.45218305332902));
#21951=CARTESIAN_POINT('Ctrl Pts',(14.7512124062873,0.178551969979598,4.4283678943965));
#21952=CARTESIAN_POINT('Ctrl Pts',(14.7433410342373,0.242559732875008,4.38839375563686));
#21953=CARTESIAN_POINT('Ctrl Pts',(14.7354696621874,0.30656749577042,4.34841961687722));
#21954=CARTESIAN_POINT('Ctrl Pts',(14.7275982901374,0.360483649899433,4.29228649829047));
#21955=CARTESIAN_POINT('Ctrl Pts',(14.7197269180875,0.397847504376097,4.22672074611392));
#21956=CARTESIAN_POINT('Ctrl Pts',(14.7118555460375,0.435211358852761,4.16115499393738));
#21957=CARTESIAN_POINT('Ctrl Pts',(14.7039841739875,0.456022913677073,4.08615660817103));
#21958=CARTESIAN_POINT('Ctrl Pts',(14.6961128019376,0.457788351878884,4.01071253147039));
#21959=CARTESIAN_POINT('Ctrl Pts',(14.6882414298876,0.459553790080695,3.93526845476975));
#21960=CARTESIAN_POINT('Ctrl Pts',(14.6803700578377,0.442273111660005,3.85937868713481));
#21961=CARTESIAN_POINT('Ctrl Pts',(14.6724986857877,0.408017034045316,3.79213698410258));
#21962=CARTESIAN_POINT('Ctrl Pts',(14.6646273137378,0.373760956430627,3.72489528107034));
#21963=CARTESIAN_POINT('Ctrl Pts',(14.6567559416878,0.32252947962194,3.6663016426408));
#21964=CARTESIAN_POINT('Ctrl Pts',(14.6488845696379,0.260461593653079,3.6233772554918));
#21965=CARTESIAN_POINT('Ctrl Pts',(14.6410131975879,0.198393707684219,3.5804528683428));
#21966=CARTESIAN_POINT('Ctrl Pts',(14.6331418255379,0.125489412555185,3.55319773247434));
#21967=CARTESIAN_POINT('Ctrl Pts',(14.625270453488,0.0504847191830214,3.54487778940425));
#21968=CARTESIAN_POINT('Ctrl Pts',(14.617399081438,-0.0245199741891427,
3.53655784633416));
#21969=CARTESIAN_POINT('Ctrl Pts',(14.6095277093881,-0.101625065804437,
3.54717309606245));
#21970=CARTESIAN_POINT('Ctrl Pts',(14.6016563373381,-0.171591169681571,
3.57545152934398));
#21971=CARTESIAN_POINT('Ctrl Pts',(14.5937849652882,-0.241557273558703,
3.6037299626255));
#21972=CARTESIAN_POINT('Ctrl Pts',(14.5859135932382,-0.304384389697674,
3.64967157946028));
#21973=CARTESIAN_POINT('Ctrl Pts',(14.5780422211883,-0.352544040227279,
3.70777126570269));
#21974=CARTESIAN_POINT('Ctrl Pts',(14.5701708491383,-0.400703690756885,
3.7658709519451));
#21975=CARTESIAN_POINT('Ctrl Pts',(14.5622994770883,-0.434195875677124,
3.83612870759516));
#21976=CARTESIAN_POINT('Ctrl Pts',(14.5544281050384,-0.449007277354457,
3.91012565253846));
#21977=CARTESIAN_POINT('Ctrl Pts',(14.5465567329884,-0.46381867903179,3.98412259748177));
#21978=CARTESIAN_POINT('Ctrl Pts',(14.5386853609385,-0.459949297466218,
4.06185873171832));
#21979=CARTESIAN_POINT('Ctrl Pts',(14.5308139888885,-0.437862794771992,
4.13401905238929));
#21980=CARTESIAN_POINT('Ctrl Pts',(14.5229426168386,-0.415776292077766,
4.20617937306026));
#21981=CARTESIAN_POINT('Ctrl Pts',(14.5150712447886,-0.375472668254887,
4.27276388016565));
#21982=CARTESIAN_POINT('Ctrl Pts',(14.5071998727387,-0.321781445311454,
4.32579385338299));
#21983=CARTESIAN_POINT('Ctrl Pts',(14.4993285006887,-0.26809022236802,4.37882382660034));
#21984=CARTESIAN_POINT('Ctrl Pts',(14.4914571286387,-0.201011400304033,
4.41829926592964));
#21985=CARTESIAN_POINT('Ctrl Pts',(14.4835857565888,-0.128582932452519,
4.43948988945229));
#21986=CARTESIAN_POINT('Ctrl Pts',(14.4790557405542,-0.0868999680795747,
4.45168520479633));
#21987=CARTESIAN_POINT('Ctrl Pts',(14.4745257245197,-0.0434451672832877,
4.45782447382869));
#21988=CARTESIAN_POINT('Ctrl Pts',(14.4699957084852,4.96934848862042E-6,
4.4578413260902));
#21989=CARTESIAN_POINT('Ctrl Pts',(14.5800042915148,-1.58578451148518E-6,
4.45791318879952));
#21990=CARTESIAN_POINT('Ctrl Pts',(14.5801660092442,-0.00155201715944126,
4.45791349841543));
#21991=CARTESIAN_POINT('Ctrl Pts',(14.5803277269736,-0.00310244544229786,
4.45790578589721));
#21992=CARTESIAN_POINT('Ctrl Pts',(14.5804894447029,-0.0046527920161852,
4.45789003224535));
#21993=CARTESIAN_POINT('Ctrl Pts',(14.5883608167529,-0.0801136257596197,
4.45712324646747));
#21994=CARTESIAN_POINT('Ctrl Pts',(14.5962321888029,-0.155380881795201,
4.43730611368561));
#21995=CARTESIAN_POINT('Ctrl Pts',(14.6041035608528,-0.22143539919095,4.4008132908088));
#21996=CARTESIAN_POINT('Ctrl Pts',(14.6119749329028,-0.287489916586699,
4.36432046793199));
#21997=CARTESIAN_POINT('Ctrl Pts',(14.6198463049527,-0.344331695342615,
4.31115195496024));
#21998=CARTESIAN_POINT('Ctrl Pts',(14.6277176770027,-0.38514947146564,4.24767885402976));
#21999=CARTESIAN_POINT('Ctrl Pts',(14.6355890490526,-0.425967247588666,
4.18420575309928));
#22000=CARTESIAN_POINT('Ctrl Pts',(14.6434604211026,-0.4507610210788,4.11042806421008));
#22001=CARTESIAN_POINT('Ctrl Pts',(14.6513317931525,-0.45655979174196,4.03518645571321));
#22002=CARTESIAN_POINT('Ctrl Pts',(14.6592031652025,-0.462358562405121,
3.95994484721634));
#22003=CARTESIAN_POINT('Ctrl Pts',(14.6670745372524,-0.449162330241309,
3.8832393191118));
#22004=CARTESIAN_POINT('Ctrl Pts',(14.6749459093024,-0.41855237967279,3.81426137832517));
#22005=CARTESIAN_POINT('Ctrl Pts',(14.6828172813524,-0.387942429104271,
3.74528343753854));
#22006=CARTESIAN_POINT('Ctrl Pts',(14.6906886534023,-0.339918760131043,
3.68403308406983));
#22007=CARTESIAN_POINT('Ctrl Pts',(14.6985600254523,-0.280235976103336,
3.63784985464301));
#22008=CARTESIAN_POINT('Ctrl Pts',(14.7064313975022,-0.220553192075631,
3.5916666252162));
#22009=CARTESIAN_POINT('Ctrl Pts',(14.7143027695522,-0.149211292993445,
3.5605505198313));
#22010=CARTESIAN_POINT('Ctrl Pts',(14.7221741416021,-0.0747590701011626,
3.54823013427646));
#22011=CARTESIAN_POINT('Ctrl Pts',(14.7300455136521,-0.000306847208877067,
3.53590974872161));
#22012=CARTESIAN_POINT('Ctrl Pts',(14.737916885702,0.0772556994935079,3.54238508299684));
#22013=CARTESIAN_POINT('Ctrl Pts',(14.745788257752,0.148634367597872,3.5668802073009));
#22014=CARTESIAN_POINT('Ctrl Pts',(14.753659629802,0.220013035702235,3.59137533160497));
#22015=CARTESIAN_POINT('Ctrl Pts',(14.7615310018519,0.285207825208577,3.63389024593787));
#22016=CARTESIAN_POINT('Ctrl Pts',(14.7694023739019,0.336406544142474,3.68933045342307));
#22017=CARTESIAN_POINT('Ctrl Pts',(14.7772737459518,0.387605263076371,3.74477066090827));
#22018=CARTESIAN_POINT('Ctrl Pts',(14.7851451180018,0.424807911437823,3.81313616154577));
#22019=CARTESIAN_POINT('Ctrl Pts',(14.7930164900517,0.443556551112275,3.88623481973509));
#22020=CARTESIAN_POINT('Ctrl Pts',(14.8008878621017,0.462305190786727,3.9593334779244));
#22021=CARTESIAN_POINT('Ctrl Pts',(14.8087592341516,0.462599821774179,4.03716529366552));
#22022=CARTESIAN_POINT('Ctrl Pts',(14.8166306062016,0.444405141642572,4.11040380200553));
#22023=CARTESIAN_POINT('Ctrl Pts',(14.8245019782516,0.426210461510966,4.18364231034555));
#22024=CARTESIAN_POINT('Ctrl Pts',(14.8323733503015,0.389526470260302,4.25228751128446));
#22025=CARTESIAN_POINT('Ctrl Pts',(14.8402447223515,0.338748948932789,4.3081137476731));
#22026=CARTESIAN_POINT('Ctrl Pts',(14.8481160944014,0.287971427605278,4.36393998406173));
#22027=CARTESIAN_POINT('Ctrl Pts',(14.8559874664514,0.22310037620092,4.40694725590009));
#22028=CARTESIAN_POINT('Ctrl Pts',(14.8638588385013,0.151909206873508,4.43198208217373));
#22029=CARTESIAN_POINT('Ctrl Pts',(14.8692406561725,0.103234351881841,4.44909890368578));
#22030=CARTESIAN_POINT('Ctrl Pts',(14.8746224738437,0.0516050086776526,
4.45781408155485));
#22031=CARTESIAN_POINT('Ctrl Pts',(14.8800042915148,-1.01702808208336E-5,
4.45785711824254));
#22032=CARTESIAN_POINT('Origin',(12.5,0.,4.));
#22033=CARTESIAN_POINT('',(15.1,-5.60735153159594E-17,4.457875));
#22034=CARTESIAN_POINT('',(15.0699957084852,-1.05870731373636E-5,4.45788944868556));
#22035=CARTESIAN_POINT('',(12.5,-5.60735153159594E-17,4.457875));
#22036=CARTESIAN_POINT('',(15.1,-0.269165465906718,4.37040446485999));
#22037=CARTESIAN_POINT('Origin',(15.1,0.,4.));
#22038=CARTESIAN_POINT('Ctrl Pts',(15.1,-0.269173508333955,4.37043259773194));
#22039=CARTESIAN_POINT('Ctrl Pts',(15.0991842588284,-0.262849866117432,
4.37503549456412));
#22040=CARTESIAN_POINT('Ctrl Pts',(15.0983685176569,-0.256407545646713,
4.37947450812006));
#22041=CARTESIAN_POINT('Ctrl Pts',(15.0975527764853,-0.249853611926923,
4.38374199825787));
#22042=CARTESIAN_POINT('Ctrl Pts',(15.0896814044354,-0.186612411779406,
4.42492050409441));
#22043=CARTESIAN_POINT('Ctrl Pts',(15.0818100323854,-0.112978907049287,
4.45012847221118));
#22044=CARTESIAN_POINT('Ctrl Pts',(15.0739386603355,-0.0377721395608013,
4.45635245505497));
#22045=CARTESIAN_POINT('Ctrl Pts',(15.072624343052,-0.0252145379490987,
4.45739170058566));
#22046=CARTESIAN_POINT('Ctrl Pts',(15.0713100257686,-0.0126130730861363,
4.45790166433459));
#22047=CARTESIAN_POINT('Ctrl Pts',(15.0699957084852,-1.05870731373636E-5,
4.45788944868556));
#22048=CARTESIAN_POINT('Origin',(11.8752146997001,0.,4.));
#22049=CARTESIAN_POINT('',(14.9247853002999,-1.38824472118437E-5,4.62497559137666));
#22050=CARTESIAN_POINT('',(15.0252146997001,-1.44513692928093E-5,4.62501972247551));
#22051=CARTESIAN_POINT('',(11.8752146997001,-1.68747709936658E-14,4.625));
#22052=CARTESIAN_POINT('',(15.1,-0.624993681275899,4.00281040303151));
#22053=CARTESIAN_POINT('Ctrl Pts',(15.0252146997001,-1.44513692928189E-5,
4.62501972247551));
#22054=CARTESIAN_POINT('Ctrl Pts',(15.0265290169835,-0.017216861979444,
4.62503639685311));
#22055=CARTESIAN_POINT('Ctrl Pts',(15.0357147063169,-0.137433797398843,
4.62017138475037));
#22056=CARTESIAN_POINT('Ctrl Pts',(15.0527717677003,-0.355236031271534,
4.54560815721762));
#22057=CARTESIAN_POINT('Ctrl Pts',(15.0763858838501,-0.571652475026301,
4.31158258982903));
#22058=CARTESIAN_POINT('Ctrl Pts',(15.09212862795,-0.624530364890795,4.10584538053252));
#22059=CARTESIAN_POINT('Ctrl Pts',(15.1,-0.624993681275899,4.00281040303152));
#22060=CARTESIAN_POINT('',(15.1,0.314930721058197,3.46014479632612));
#22061=CARTESIAN_POINT('Origin',(15.1,0.,4.));
#22062=CARTESIAN_POINT('Ctrl Pts',(14.9247853002999,-1.38824472118368E-5,
4.62497559137666));
#22063=CARTESIAN_POINT('Ctrl Pts',(14.9272748546787,-0.0326052931943186,
4.62500276606431));
#22064=CARTESIAN_POINT('Ctrl Pts',(14.9376357811074,-0.168225686180582,
4.61457389311938));
#22065=CARTESIAN_POINT('Ctrl Pts',(14.9558680795861,-0.394527586443172,
4.517903766532));
#22066=CARTESIAN_POINT('Ctrl Pts',(14.979482195736,-0.593077772790822,4.26857965265179));
#22067=CARTESIAN_POINT('Ctrl Pts',(15.0030963118859,-0.649493436571599,
3.95488773069898));
#22068=CARTESIAN_POINT('Ctrl Pts',(15.0267104280357,-0.550252000240565,
3.65200904506483));
#22069=CARTESIAN_POINT('Ctrl Pts',(15.0503245441856,-0.319142060764588,
3.43252503194012));
#22070=CARTESIAN_POINT('Ctrl Pts',(15.0739386603355,-0.0115409051696555,
3.34904846156061));
#22071=CARTESIAN_POINT('Ctrl Pts',(15.0904971456069,0.20608092381284,3.39989411918499));
#22072=CARTESIAN_POINT('Ctrl Pts',(15.0991842588284,0.305720220830039,3.45471854406458));
#22073=CARTESIAN_POINT('Ctrl Pts',(15.1,0.314937815442301,3.46010549098218));
#22074=CARTESIAN_POINT('Origin',(11.8752146997001,0.,4.));
#22075=CARTESIAN_POINT('',(14.6247853002999,-2.16459804047719E-6,4.62505212776347));
#22076=CARTESIAN_POINT('',(14.7252146997001,1.17863019661874E-5,4.62503218402409));
#22077=CARTESIAN_POINT('',(11.8752146997001,-1.68747709936658E-14,4.625));
#22078=CARTESIAN_POINT('Ctrl Pts',(14.7252146997001,1.17863019662174E-5,
4.62503218402409));
#22079=CARTESIAN_POINT('Ctrl Pts',(14.7320725523841,-0.0897427467603322,
4.62495430540108));
#22080=CARTESIAN_POINT('Ctrl Pts',(14.746801777118,-0.282587126126967,4.58296482291278));
#22081=CARTESIAN_POINT('Ctrl Pts',(14.7694023739019,-0.520130285395982,
4.39158760667368));
#22082=CARTESIAN_POINT('Ctrl Pts',(14.7930164900517,-0.64367318065081,4.09778141619902));
#22083=CARTESIAN_POINT('Ctrl Pts',(14.8166306062016,-0.612955311082805,
3.78054123783642));
#22084=CARTESIAN_POINT('Ctrl Pts',(14.8402447223515,-0.435338447621071,
3.51589585985611));
#22085=CARTESIAN_POINT('Ctrl Pts',(14.8638588385013,-0.153389665944836,
3.36726945127358));
#22086=CARTESIAN_POINT('Ctrl Pts',(14.8874729546512,0.165319955489652,3.37028123293502));
#22087=CARTESIAN_POINT('Ctrl Pts',(14.9110870708011,0.444409630539555,3.52420969451069));
#22088=CARTESIAN_POINT('Ctrl Pts',(14.9347011869509,0.616993161964042,3.79216419995926));
#22089=CARTESIAN_POINT('Ctrl Pts',(14.9583153031008,0.641710593195818,4.10992889087348));
#22090=CARTESIAN_POINT('Ctrl Pts',(14.9819294192507,0.512636325700993,4.40134645341462));
#22091=CARTESIAN_POINT('Ctrl Pts',(15.0042292181171,0.274729866520086,4.58571614948967));
#22092=CARTESIAN_POINT('Ctrl Pts',(15.0186576449336,0.0858074045169303,
4.62493653494651));
#22093=CARTESIAN_POINT('Ctrl Pts',(15.0252146997001,-1.44513692928189E-5,
4.62501972247551));
#22094=CARTESIAN_POINT('Ctrl Pts',(14.6247853002999,-2.16459804049194E-6,
4.62505212776347));
#22095=CARTESIAN_POINT('Ctrl Pts',(14.6249470180292,-0.00211850554115318,
4.62505255038961));
#22096=CARTESIAN_POINT('Ctrl Pts',(14.6329801078086,-0.107244412024774,
4.62452960748548));
#22097=CARTESIAN_POINT('Ctrl Pts',(14.6488845696379,-0.314835022974042,
4.56987302880665));
#22098=CARTESIAN_POINT('Ctrl Pts',(14.6724986857877,-0.547602339746838,
4.35214775046202));
#22099=CARTESIAN_POINT('Ctrl Pts',(14.6961128019376,-0.649132943719538,
4.05002781234082));
#22100=CARTESIAN_POINT('Ctrl Pts',(14.7197269180875,-0.595094318970103,
3.73591836064326));
#22101=CARTESIAN_POINT('Ctrl Pts',(14.7433410342373,-0.398437197867616,
3.48509791236843));
#22102=CARTESIAN_POINT('Ctrl Pts',(14.7669551503872,-0.1062918289807,3.35767733339665));
#22103=CARTESIAN_POINT('Ctrl Pts',(14.7905692665371,0.211327117384507,3.38419385377023));
#22104=CARTESIAN_POINT('Ctrl Pts',(14.8141833826869,0.478300047385911,3.5582926020622));
#22105=CARTESIAN_POINT('Ctrl Pts',(14.8377974988368,0.630645044771057,3.83824960712979));
#22106=CARTESIAN_POINT('Ctrl Pts',(14.8614116149867,0.631851559871185,4.15697121131127));
#22107=CARTESIAN_POINT('Ctrl Pts',(14.8850257311365,0.481630465478622,4.4380735902585));
#22108=CARTESIAN_POINT('Ctrl Pts',(14.9061502929076,0.243989509668873,4.59562135563586));
#22109=CARTESIAN_POINT('Ctrl Pts',(14.9194034826287,0.0704409072858971,
4.62491684623921));
#22110=CARTESIAN_POINT('Ctrl Pts',(14.9247853002999,-1.38824472118368E-5,
4.62497559137666));
#22111=CARTESIAN_POINT('Origin',(11.8752146997001,0.,4.));
#22112=CARTESIAN_POINT('',(14.3247853002999,1.51969053300144E-5,4.6249871875462));
#22113=CARTESIAN_POINT('',(14.4252146997001,6.78316748347314E-6,4.62495403506715));
#22114=CARTESIAN_POINT('',(11.8752146997001,-1.68747709936658E-14,4.625));
#22115=CARTESIAN_POINT('Ctrl Pts',(14.4252146997001,6.78316748347826E-6,
4.62495403506715));
#22116=CARTESIAN_POINT('Ctrl Pts',(14.4297447157347,-0.0593027126443913,
4.62493103170719));
#22117=CARTESIAN_POINT('Ctrl Pts',(14.4421461038192,-0.221686029527806,
4.60198961095629));
#22118=CARTESIAN_POINT('Ctrl Pts',(14.4624188639536,-0.457506203155893,
4.46321101183598));
#22119=CARTESIAN_POINT('Ctrl Pts',(14.4860329801035,-0.622549707754089,
4.19054718257559));
#22120=CARTESIAN_POINT('Ctrl Pts',(14.5096470962533,-0.63839484111024,3.87221739454711));
#22121=CARTESIAN_POINT('Ctrl Pts',(14.5332612124032,-0.501244206711231,
3.58451159745434));
#22122=CARTESIAN_POINT('Ctrl Pts',(14.5568753285531,-0.243966908844842,
3.39638048838484));
#22123=CARTESIAN_POINT('Ctrl Pts',(14.5804894447029,0.0717787570654544,
3.35291099727801));
#22124=CARTESIAN_POINT('Ctrl Pts',(14.6041035608528,0.370322144162233,3.46452089026927));
#22125=CARTESIAN_POINT('Ctrl Pts',(14.6277176770027,0.580115251486915,3.70446207957941));
#22126=CARTESIAN_POINT('Ctrl Pts',(14.6513317931525,0.650879700384091,4.0152309888134));
#22127=CARTESIAN_POINT('Ctrl Pts',(14.6749459093024,0.565656298155129,4.32234968564526));
#22128=CARTESIAN_POINT('Ctrl Pts',(14.6985600254523,0.344869426209941,4.55221503612336));
#22129=CARTESIAN_POINT('Ctrl Pts',(14.7153162889182,0.129554394067723,4.62141618582314));
#22130=CARTESIAN_POINT('Ctrl Pts',(14.7242011803341,0.0132765736394338,
4.62504369367533));
#22131=CARTESIAN_POINT('Ctrl Pts',(14.7252146997001,1.17863019662174E-5,
4.62503218402409));
#22132=CARTESIAN_POINT('Ctrl Pts',(14.3247853002999,1.51969053300109E-5,
4.6249871875462));
#22133=CARTESIAN_POINT('Ctrl Pts',(14.3304905534298,-0.0746697890657793,
4.62491698721088));
#22134=CARTESIAN_POINT('Ctrl Pts',(14.3440671786096,-0.252453835406249,
4.59302599116618));
#22135=CARTESIAN_POINT('Ctrl Pts',(14.3655151758395,-0.490432948250941,
4.42819608115853));
#22136=CARTESIAN_POINT('Ctrl Pts',(14.3891292919893,-0.634910852255616,
4.14409916841427));
#22137=CARTESIAN_POINT('Ctrl Pts',(14.4127434081392,-0.627227950688033,
3.82546788683648));
#22138=CARTESIAN_POINT('Ctrl Pts',(14.4363575242891,-0.469225504392149,
3.54866444115539));
#22139=CARTESIAN_POINT('Ctrl Pts',(14.4599716404389,-0.198769899531221,
3.38002670405092));
#22140=CARTESIAN_POINT('Ctrl Pts',(14.4835857565888,0.11932229545683,3.35996988316441));
#22141=CARTESIAN_POINT('Ctrl Pts',(14.5071998727387,0.408818071695872,3.49330073524378));
#22142=CARTESIAN_POINT('Ctrl Pts',(14.5308139888885,0.600337751131954,3.74806559342675));
#22143=CARTESIAN_POINT('Ctrl Pts',(14.5544281050384,0.647982309355475,4.06320828594604));
#22144=CARTESIAN_POINT('Ctrl Pts',(14.5780422211883,0.540333396317157,4.36320267272319));
#22145=CARTESIAN_POINT('Ctrl Pts',(14.6014946196088,0.304813865567294,4.57469465218781));
#22146=CARTESIAN_POINT('Ctrl Pts',(14.6170756459793,0.100891269655612,4.62503197968527));
#22147=CARTESIAN_POINT('Ctrl Pts',(14.6247853002999,-2.16459804049194E-6,
4.62505212776347));
#22148=CARTESIAN_POINT('Origin',(11.8752146997001,0.,4.));
#22149=CARTESIAN_POINT('',(14.0247853002999,-6.3966029390794E-6,4.62495348172753));
#22150=CARTESIAN_POINT('',(14.1252146997001,-1.50974863142078E-5,4.62498583382255));
#22151=CARTESIAN_POINT('',(11.8752146997001,-1.68747709936658E-14,4.625));
#22152=CARTESIAN_POINT('Ctrl Pts',(14.1252146997001,-1.50974863141889E-5,
4.62498583382255));
#22153=CARTESIAN_POINT('Ctrl Pts',(14.1274168790852,-0.0288430498503269,
4.62501265364587));
#22154=CARTESIAN_POINT('Ctrl Pts',(14.1374904305203,-0.160695812902997,
4.61605202430223));
#22155=CARTESIAN_POINT('Ctrl Pts',(14.1554353540053,-0.385112282251534,
4.52494275637564));
#22156=CARTESIAN_POINT('Ctrl Pts',(14.1790494701552,-0.588131968915973,
4.27924389796604));
#22157=CARTESIAN_POINT('Ctrl Pts',(14.2026635863051,-0.65020173504413,3.96662229549764));
#22158=CARTESIAN_POINT('Ctrl Pts',(14.2262777024549,-0.556446129094758,
3.66199989226673));
#22159=CARTESIAN_POINT('Ctrl Pts',(14.2498918186048,-0.329334334698108,
3.43838156778717));
#22160=CARTESIAN_POINT('Ctrl Pts',(14.2735059347547,-0.0232952743833569,
3.34935901020328));
#22161=CARTESIAN_POINT('Ctrl Pts',(14.2971200509045,0.28832666060365,3.41626709515619));
#22162=CARTESIAN_POINT('Ctrl Pts',(14.3207341670544,0.530849104237583,3.62307083431711));
#22163=CARTESIAN_POINT('Ctrl Pts',(14.3443482832043,0.646149864620809,3.92020827196535));
#22164=CARTESIAN_POINT('Ctrl Pts',(14.3679623993541,0.606596311879891,4.2364683526943));
#22165=CARTESIAN_POINT('Ctrl Pts',(14.391576515504,0.42166773027486,4.49605714656388));
#22166=CARTESIAN_POINT('Ctrl Pts',(14.4106606156193,0.190545343529355,4.60977018898031));
#22167=CARTESIAN_POINT('Ctrl Pts',(14.4218733436847,0.0437536792250838,
4.62497100242767));
#22168=CARTESIAN_POINT('Ctrl Pts',(14.4252146997001,6.78316748347826E-6,
4.62495403506715));
#22169=CARTESIAN_POINT('Ctrl Pts',(14.0247853002999,-6.39660293913491E-6,
4.62495348172753));
#22170=CARTESIAN_POINT('Ctrl Pts',(14.0281627167804,-0.0442255271350925,
4.62496963662755));
#22171=CARTESIAN_POINT('Ctrl Pts',(14.0394115053108,-0.191490205391595,
4.6095527480466));
#22172=CARTESIAN_POINT('Ctrl Pts',(14.0585316658912,-0.422790583021024,
4.49510047824495));
#22173=CARTESIAN_POINT('Ctrl Pts',(14.0821457820411,-0.60713052675338,4.23509335195577));
#22174=CARTESIAN_POINT('Ctrl Pts',(14.1057598981909,-0.645967413308333,
3.91874446730605));
#22175=CARTESIAN_POINT('Ctrl Pts',(14.1293740143408,-0.529993712466286,
3.62186903671368));
#22176=CARTESIAN_POINT('Ctrl Pts',(14.1529881304907,-0.287003328966194,
3.41561532377041));
#22177=CARTESIAN_POINT('Ctrl Pts',(14.1766022466405,0.0247694002478971,
3.34941346658496));
#22178=CARTESIAN_POINT('Ctrl Pts',(14.2002163627904,0.330605970264406,3.43912920108534));
#22179=CARTESIAN_POINT('Ctrl Pts',(14.2238304789403,0.557210518047066,3.66326152695696));
#22180=CARTESIAN_POINT('Ctrl Pts',(14.2474445950901,0.650275686248857,3.96809557204375));
#22181=CARTESIAN_POINT('Ctrl Pts',(14.27105871124,0.587497759452106,4.28057573538778));
#22182=CARTESIAN_POINT('Ctrl Pts',(14.2946728273899,0.383921904832036,4.52581397056352));
#22183=CARTESIAN_POINT('Ctrl Pts',(14.3125816904098,0.159750963363977,4.61623247111552));
#22184=CARTESIAN_POINT('Ctrl Pts',(14.3226191813798,0.0283709170587055,
4.62501384057475));
#22185=CARTESIAN_POINT('Ctrl Pts',(14.3247853002999,1.51969053300109E-5,
4.6249871875462));
#22186=CARTESIAN_POINT('Origin',(11.8752146997001,0.,4.));
#22187=CARTESIAN_POINT('',(13.7247853002999,-1.20831421157597E-5,4.62503091248755));
#22188=CARTESIAN_POINT('',(13.8252146997001,1.68461488569462E-6,4.62505238998457));
#22189=CARTESIAN_POINT('',(11.8752146997001,-1.68747709936658E-14,4.625));
#22190=CARTESIAN_POINT('Ctrl Pts',(13.8252146997001,1.68461488569581E-6,
4.62505238998457));
#22191=CARTESIAN_POINT('Ctrl Pts',(13.8329604144858,-0.101363538932993,
4.62503644193381));
#22192=CARTESIAN_POINT('Ctrl Pts',(13.8485775013214,-0.305753798836605,
4.57432856173903));
#22193=CARTESIAN_POINT('Ctrl Pts',(13.8720659602069,-0.541154937947787,
4.36197748624323));
#22194=CARTESIAN_POINT('Ctrl Pts',(13.8956800763568,-0.648123865072376,
4.06173996222779));
#22195=CARTESIAN_POINT('Ctrl Pts',(13.9192941925067,-0.599765396122921,
3.74670602647169));
#22196=CARTESIAN_POINT('Ctrl Pts',(13.9429083086565,-0.407668974822819,
3.49237575473668));
#22197=CARTESIAN_POINT('Ctrl Pts',(13.9665224248064,-0.117871845784803,
3.35970116712309));
#22198=CARTESIAN_POINT('Ctrl Pts',(13.9901365409563,0.200174091641329,3.38047865214521));
#22199=CARTESIAN_POINT('Ctrl Pts',(14.0137506571061,0.470246914526057,3.54972874087838));
#22200=CARTESIAN_POINT('Ctrl Pts',(14.037364773256,0.627621790796785,3.82688947135059));
#22201=CARTESIAN_POINT('Ctrl Pts',(14.0609788894059,0.634582735815489,4.14553734509456));
#22202=CARTESIAN_POINT('Ctrl Pts',(14.0845930055557,0.489461510650943,4.42930618095194));
#22203=CARTESIAN_POINT('Ctrl Pts',(14.1060049423205,0.251510284961593,4.59332024860173));
#22204=CARTESIAN_POINT('Ctrl Pts',(14.1195455070353,0.074198300926532,4.62491679006221));
#22205=CARTESIAN_POINT('Ctrl Pts',(14.1252146997001,-1.50974863141889E-5,
4.62498583382255));
#22206=CARTESIAN_POINT('Ctrl Pts',(13.7247853002999,-1.20831421156938E-5,
4.62503091248755));
#22207=CARTESIAN_POINT('Ctrl Pts',(13.7258348801309,-0.013748904810447,
4.62504304225186));
#22208=CARTESIAN_POINT('Ctrl Pts',(13.734755832012,-0.130498998332177,4.62127102305724));
#22209=CARTESIAN_POINT('Ctrl Pts',(13.7515481559429,-0.346119716157775,
4.55143222859795));
#22210=CARTESIAN_POINT('Ctrl Pts',(13.7751622720928,-0.566385203513325,
4.32106722332061));
#22211=CARTESIAN_POINT('Ctrl Pts',(13.7987763882427,-0.650912534047929,
4.01375622291695));
#22212=CARTESIAN_POINT('Ctrl Pts',(13.8223905043925,-0.57944414457563,3.70314844792952));
#22213=CARTESIAN_POINT('Ctrl Pts',(13.8460046205424,-0.369107932149097,
3.46368321387984));
#22214=CARTESIAN_POINT('Ctrl Pts',(13.8696187366923,-0.0703124342978696,
3.35275003110641));
#22215=CARTESIAN_POINT('Ctrl Pts',(13.8932328528421,0.245333927901481,3.3969348091043));
#22216=CARTESIAN_POINT('Ctrl Pts',(13.916846968992,0.502184306426786,3.58564835824111));
#22217=CARTESIAN_POINT('Ctrl Pts',(13.9404610851419,0.638682720042094,3.87366416276737));
#22218=CARTESIAN_POINT('Ctrl Pts',(13.9640752012917,0.62211637371287,4.19195723015293));
#22219=CARTESIAN_POINT('Ctrl Pts',(13.9876893174416,0.456455507660852,4.46424641105313));
#22220=CARTESIAN_POINT('Ctrl Pts',(14.007926017111,0.220741531225703,4.60224444133776));
#22221=CARTESIAN_POINT('Ctrl Pts',(14.0202913447304,0.058831122868106,4.62493198618401));
#22222=CARTESIAN_POINT('Ctrl Pts',(14.0247853002999,-6.39660293913491E-6,
4.62495348172753));
#22223=CARTESIAN_POINT('Origin',(11.8752146997001,0.,4.));
#22224=CARTESIAN_POINT('',(13.4247853002999,1.36962628664028E-5,4.62502243215823));
#22225=CARTESIAN_POINT('',(13.5252146997001,1.40828270379035E-5,4.62497680637469));
#22226=CARTESIAN_POINT('',(11.8752146997001,-1.68747709936658E-14,4.625));
#22227=CARTESIAN_POINT('Ctrl Pts',(13.5252146997001,1.4082827037902E-5,
4.62497680637469));
#22228=CARTESIAN_POINT('Ctrl Pts',(13.5306325778363,-0.0709123884867814,
4.62491668074428));
#22229=CARTESIAN_POINT('Ctrl Pts',(13.5439218280225,-0.244933372371362,
4.59533688876844));
#22230=CARTESIAN_POINT('Ctrl Pts',(13.5650824502587,-0.482621788093898,
4.43698120905743));
#22231=CARTESIAN_POINT('Ctrl Pts',(13.5886965664085,-0.632205603168059,
4.15553919999523));
#22232=CARTESIAN_POINT('Ctrl Pts',(13.6123106825584,-0.630276944445953,
3.83682113889318));
#22233=CARTESIAN_POINT('Ctrl Pts',(13.6359247987083,-0.477298028416376,
3.55721002779864));
#22234=CARTESIAN_POINT('Ctrl Pts',(13.6595389148582,-0.209931317243796,
3.38371661595291));
#22235=CARTESIAN_POINT('Ctrl Pts',(13.683153031008,0.107746895509167,3.35791980725116));
#22236=CARTESIAN_POINT('Ctrl Pts',(13.7067671471579,0.399602814690774,3.48600198647908));
#22237=CARTESIAN_POINT('Ctrl Pts',(13.7303812633077,0.59569113756138,3.73726736776131));
#22238=CARTESIAN_POINT('Ctrl Pts',(13.7539953794576,0.649017932507905,4.05149845333026));
#22239=CARTESIAN_POINT('Ctrl Pts',(13.7776094956075,0.546803061895555,4.35338757606046));
#22240=CARTESIAN_POINT('Ctrl Pts',(13.8012236117573,0.313543031018869,4.57058490613733));
#22241=CARTESIAN_POINT('Ctrl Pts',(13.8170920131216,0.106300066848774,4.6246481407235));
#22242=CARTESIAN_POINT('Ctrl Pts',(13.8250890424358,0.00164611344283092,
4.62505264870678));
#22243=CARTESIAN_POINT('Ctrl Pts',(13.8252146997001,1.68461488569581E-6,
4.62505238998457));
#22244=CARTESIAN_POINT('Ctrl Pts',(13.4247853002999,1.36962628664097E-5,
4.62502243215823));
#22245=CARTESIAN_POINT('Ctrl Pts',(13.4313784155315,-0.086279884022628,
4.62493973056585));
#22246=CARTESIAN_POINT('Ctrl Pts',(13.445842902813,-0.275670893367246,4.58538934244717));
#22247=CARTESIAN_POINT('Ctrl Pts',(13.4681787621445,-0.513544980480383,
4.40018484937968));
#22248=CARTESIAN_POINT('Ctrl Pts',(13.4917928782944,-0.64195771209056,4.10847422061066));
#22249=CARTESIAN_POINT('Ctrl Pts',(13.5154069944443,-0.616520809113462,
3.79076698974655));
#22250=CARTESIAN_POINT('Ctrl Pts',(13.5390211105941,-0.443330402422436,
3.52320390633144));
#22251=CARTESIAN_POINT('Ctrl Pts',(13.562635226744,-0.163892778617988,3.36990832590288));
#22252=CARTESIAN_POINT('Ctrl Pts',(13.5862493428939,0.154822890495328,3.36761860145296));
#22253=CARTESIAN_POINT('Ctrl Pts',(13.6098634590437,0.43643417612693,3.51688348138565));
#22254=CARTESIAN_POINT('Ctrl Pts',(13.6334775751936,0.613450973283793,3.78193059814177));
#22255=CARTESIAN_POINT('Ctrl Pts',(13.6570916913435,0.643449974253473,4.09923956510808));
#22256=CARTESIAN_POINT('Ctrl Pts',(13.6807058074933,0.519241709620395,4.39276507945606));
#22257=CARTESIAN_POINT('Ctrl Pts',(13.7032703438121,0.281645253009076,4.58329909926801));
#22258=CARTESIAN_POINT('Ctrl Pts',(13.717963508081,0.0892710189108511,4.62495207452848));
#22259=CARTESIAN_POINT('Ctrl Pts',(13.7247853002999,-1.20831421156938E-5,
4.62503091248755));
#22260=CARTESIAN_POINT('Origin',(11.8752146997001,0.,4.));
#22261=CARTESIAN_POINT('',(13.1247853002999,3.84888821539087E-6,4.62495078081483));
#22262=CARTESIAN_POINT('',(13.2252146997001,-9.32440196476731E-6,4.62495874418382));
#22263=CARTESIAN_POINT('',(11.8752146997001,-1.68747709936658E-14,4.625));
#22264=CARTESIAN_POINT('Ctrl Pts',(13.2252146997001,-9.32440196474427E-6,
4.62495874418382));
#22265=CARTESIAN_POINT('Ctrl Pts',(13.2283047411869,-0.040464997295585,
4.62498052751194));
#22266=CARTESIAN_POINT('Ctrl Pts',(13.2392661547237,-0.18396024524725,4.61125364372682));
#22267=CARTESIAN_POINT('Ctrl Pts',(13.2580989403104,-0.413782468289504,
4.50265339583901));
#22268=CARTESIAN_POINT('Ctrl Pts',(13.2817130564603,-0.602786876612853,
4.24601696851145));
#22269=CARTESIAN_POINT('Ctrl Pts',(13.3053271726101,-0.647329213752593,
3.9304208620728));
#22270=CARTESIAN_POINT('Ctrl Pts',(13.32894128876,-0.536734598538914,3.6314998804023));
#22271=CARTESIAN_POINT('Ctrl Pts',(13.3525554049099,-0.297507800394296,
3.42089251764738));
#22272=CARTESIAN_POINT('Ctrl Pts',(13.3761695210598,0.0130188131672444,
3.34907229440132));
#22273=CARTESIAN_POINT('Ctrl Pts',(13.3997836372096,0.320425377524893,3.43325142712992));
#22274=CARTESIAN_POINT('Ctrl Pts',(13.4233977533595,0.551039769569266,3.65325580067535));
#22275=CARTESIAN_POINT('Ctrl Pts',(13.4470118695093,0.649593644862141,3.95635983539258));
#22276=CARTESIAN_POINT('Ctrl Pts',(13.4706259856592,0.592467881122722,4.26992253935193));
#22277=CARTESIAN_POINT('Ctrl Pts',(13.4942401018091,0.393353065302923,4.5187964277335));
#22278=CARTESIAN_POINT('Ctrl Pts',(13.5124363398227,0.1672808180195,4.61476328251587));
#22279=CARTESIAN_POINT('Ctrl Pts',(13.5227612057864,0.0321332374692893,
4.62500403435298));
#22280=CARTESIAN_POINT('Ctrl Pts',(13.5252146997001,1.4082827037902E-5,
4.62497680637469));
#22281=CARTESIAN_POINT('Ctrl Pts',(13.1247853002999,3.84888821536311E-6,
4.62495078081483));
#22282=CARTESIAN_POINT('Ctrl Pts',(13.1290505788821,-0.0558403875021823,
4.6249385719914));
#22283=CARTESIAN_POINT('Ctrl Pts',(13.1411872295142,-0.214751600407627,
4.60383286368317));
#22284=CARTESIAN_POINT('Ctrl Pts',(13.1611952521963,-0.449738236712957,
4.47075670902068));
#22285=CARTESIAN_POINT('Ctrl Pts',(13.1848093683461,-0.619294173608025,
4.2008758003961));
#22286=CARTESIAN_POINT('Ctrl Pts',(13.208423484496,-0.64043195068177,3.88285360784221));
#22287=CARTESIAN_POINT('Ctrl Pts',(13.2320376006459,-0.508085752511173,
3.59290636366459));
#22288=CARTESIAN_POINT('Ctrl Pts',(13.2556517167957,-0.253973266794505,
3.40052194335125));
#22289=CARTESIAN_POINT('Ctrl Pts',(13.2792658329456,0.0610056803032868,
3.3518066124833));
#22290=CARTESIAN_POINT('Ctrl Pts',(13.3028799490955,0.361364191435218,3.45843533922715));
#22291=CARTESIAN_POINT('Ctrl Pts',(13.3264940652453,0.575119258511334,3.69485380694));
#22292=CARTESIAN_POINT('Ctrl Pts',(13.3501081813952,0.65104299168552,4.00440268404554));
#22293=CARTESIAN_POINT('Ctrl Pts',(13.3737222975451,0.570939739771795,4.31289642727099));
#22294=CARTESIAN_POINT('Ctrl Pts',(13.3973364136949,0.354006804717113,4.54640236352309));
#22295=CARTESIAN_POINT('Ctrl Pts',(13.4143574146132,0.136489422610972,4.62032507485564));
#22296=CARTESIAN_POINT('Ctrl Pts',(13.4235070434815,0.0167440814458925,
4.62503846613771));
#22297=CARTESIAN_POINT('Ctrl Pts',(13.4247853002999,1.36962628664097E-5,
4.62502243215823));
#22298=CARTESIAN_POINT('Origin',(11.8752146997001,0.,4.));
#22299=CARTESIAN_POINT('',(12.8247853002999,-1.55438223423121E-5,4.62499607812274));
#22300=CARTESIAN_POINT('',(12.9252146997001,-9.4222586321007E-6,4.62504029123831));
#22301=CARTESIAN_POINT('',(11.8752146997001,-1.68747709936658E-14,4.625));
#22302=CARTESIAN_POINT('Ctrl Pts',(12.9252146997001,-9.42225863212465E-6,
4.62504029123832));
#22303=CARTESIAN_POINT('Ctrl Pts',(12.9259769045375,-0.00998466834883174,
4.6250476064301));
#22304=CARTESIAN_POINT('Ctrl Pts',(12.9346104814248,-0.122971475467856,
4.62239759066569));
#22305=CARTESIAN_POINT('Ctrl Pts',(12.9511154303622,-0.336107011072318,
4.55759164674784));
#22306=CARTESIAN_POINT('Ctrl Pts',(12.974729546512,-0.56049590900091,4.33124115596169));
#22307=CARTESIAN_POINT('Ctrl Pts',(12.9983436626619,-0.650558060547343,
4.02550641626558));
#22308=CARTESIAN_POINT('Ctrl Pts',(13.0219577788117,-0.584709444123524,
3.71365888635357));
#22309=CARTESIAN_POINT('Ctrl Pts',(13.0455718949616,-0.378731139057797,
3.47043499764384));
#22310=CARTESIAN_POINT('Ctrl Pts',(13.0691860111115,-0.0819872800401352,
3.35412504823007));
#22311=CARTESIAN_POINT('Ctrl Pts',(13.0928001272613,0.234405401379786,3.39260352716186));
#22312=CARTESIAN_POINT('Ctrl Pts',(13.1164142434112,0.494621196584012,3.57664879910166));
#22313=CARTESIAN_POINT('Ctrl Pts',(13.1400283595611,0.636297578801308,3.86215313342763));
#22314=CARTESIAN_POINT('Ctrl Pts',(13.1636424757109,0.625480816776257,4.18069342892634));
#22315=CARTESIAN_POINT('Ctrl Pts',(13.1872565918608,0.464763222827219,4.45592928631477));
#22316=CARTESIAN_POINT('Ctrl Pts',(13.2077806665239,0.228267895462889,4.60018049807294));
#22317=CARTESIAN_POINT('Ctrl Pts',(13.220433369137,0.0625891701764018,4.62492503806923));
#22318=CARTESIAN_POINT('Ctrl Pts',(13.2252146997001,-9.32440196474427E-6,
4.62495874418382));
#22319=CARTESIAN_POINT('Ctrl Pts',(12.8247853002999,-1.55438223423052E-5,
4.62499607812274));
#22320=CARTESIAN_POINT('Ctrl Pts',(12.8267227422326,-0.0253767156259869,
4.62502109614712));
#22321=CARTESIAN_POINT('Ctrl Pts',(12.8365315562153,-0.153759343851268,
4.61735081595804));
#22322=CARTESIAN_POINT('Ctrl Pts',(12.854211742248,-0.376327535803878,4.5312757721487));
#22323=CARTESIAN_POINT('Ctrl Pts',(12.8778258583979,-0.583405888470749,
4.28898776831928));
#22324=CARTESIAN_POINT('Ctrl Pts',(12.9014399745477,-0.650666957548692,
3.97744183415536));
#22325=CARTESIAN_POINT('Ctrl Pts',(12.9250540906976,-0.561991161265395,
3.67130212143154));
#22326=CARTESIAN_POINT('Ctrl Pts',(12.9486682068475,-0.338630270727757,
3.44393714350224));
#22327=CARTESIAN_POINT('Ctrl Pts',(12.9722823229973,-0.0341142786054444,
3.34983650006563));
#22328=CARTESIAN_POINT('Ctrl Pts',(12.9958964391472,0.278577437919422,3.41155206540036));
#22329=CARTESIAN_POINT('Ctrl Pts',(13.0195105552971,0.524506132150044,3.61429327464512));
#22330=CARTESIAN_POINT('Ctrl Pts',(13.0431246714469,0.644733280558021,3.90947178565704));
#22331=CARTESIAN_POINT('Ctrl Pts',(13.0667387875968,0.61044561006836,4.22634601343335));
#22332=CARTESIAN_POINT('Ctrl Pts',(13.0903529037467,0.429860399609997,4.4889748434194));
#22333=CARTESIAN_POINT('Ctrl Pts',(13.1097017413144,0.197481915229314,4.60814700801091));
#22334=CARTESIAN_POINT('Ctrl Pts',(13.1211792068321,0.0472175377905832,
4.6249611028038));
#22335=CARTESIAN_POINT('Ctrl Pts',(13.1247853002999,3.84888821536311E-6,
4.62495078081483));
#22336=CARTESIAN_POINT('Origin',(11.8752146997001,0.,4.));
#22337=CARTESIAN_POINT('',(12.5247853002999,3.80998376854277E-6,4.62503871776264));
#22338=CARTESIAN_POINT('',(12.6252146997001,1.49489494596481E-5,4.6250110476872));
#22339=CARTESIAN_POINT('',(11.8752146997001,-1.68747709936658E-14,4.625));
#22340=CARTESIAN_POINT('',(12.5,0.310062960217711,4.54266560670548));
#22341=CARTESIAN_POINT('Ctrl Pts',(12.5,0.310062960217722,4.54266560670548));
#22342=CARTESIAN_POINT('Ctrl Pts',(12.50787137205,0.220600394030941,4.59378185169648));
#22343=CARTESIAN_POINT('Ctrl Pts',(12.5161331388166,0.113220056708515,4.6237347594226));
#22344=CARTESIAN_POINT('Ctrl Pts',(12.5243949055832,0.00511234815255113,
4.6250406321328));
#22345=CARTESIAN_POINT('Ctrl Pts',(12.5247853002999,3.80998376856706E-6,
4.62503871776264));
#22346=CARTESIAN_POINT('',(12.5,0.310062960217774,3.45733439329455));
#22347=CARTESIAN_POINT('Origin',(12.5,0.,4.));
#22348=CARTESIAN_POINT('Ctrl Pts',(12.5,0.310093463203755,3.45730861053195));
#22349=CARTESIAN_POINT('Ctrl Pts',(12.5008157411716,0.319367492808711,3.46259780682489));
#22350=CARTESIAN_POINT('Ctrl Pts',(12.5095028543931,0.416666480413896,3.52147574364868));
#22351=CARTESIAN_POINT('Ctrl Pts',(12.5260613396645,0.569511032758309,3.68451895614546));
#22352=CARTESIAN_POINT('Ctrl Pts',(12.5496754558144,0.651018771792273,3.99264764559437));
#22353=CARTESIAN_POINT('Ctrl Pts',(12.5732895719643,0.576495013506714,4.3025367374363));
#22354=CARTESIAN_POINT('Ctrl Pts',(12.5969036881141,0.363815091701307,4.53992168461618));
#22355=CARTESIAN_POINT('Ctrl Pts',(12.6142120640261,0.144017971622128,4.61907377583531));
#22356=CARTESIAN_POINT('Ctrl Pts',(12.6236490678881,0.0205077016108913,
4.62503160004571));
#22357=CARTESIAN_POINT('Ctrl Pts',(12.6252146997001,1.49489494596471E-5,
4.6250110476872));
#22358=CARTESIAN_POINT('Origin',(11.8752146997001,0.,4.));
#22359=CARTESIAN_POINT('Ctrl Pts',(12.6252146997001,1.49489494596471E-5,
4.6250110476872));
#22360=CARTESIAN_POINT('Ctrl Pts',(12.631520439938,-0.0825216819810338,
4.62492827098767));
#22361=CARTESIAN_POINT('Ctrl Pts',(12.6456975522259,-0.268159494659544,
4.5879440580038));
#22362=CARTESIAN_POINT('Ctrl Pts',(12.6677460365637,-0.506235857616531,
4.40939182910775));
#22363=CARTESIAN_POINT('Ctrl Pts',(12.6913601527136,-0.639894509617229,
4.12004729681268));
#22364=CARTESIAN_POINT('Ctrl Pts',(12.7149742688635,-0.620198095551099,
3.8019325752266));
#22365=CARTESIAN_POINT('Ctrl Pts',(12.7385883850133,-0.451866840211785,
3.53128609963859));
#22366=CARTESIAN_POINT('Ctrl Pts',(12.7622025011632,-0.17524257447904,3.37297016902465));
#22367=CARTESIAN_POINT('Ctrl Pts',(12.7858166173131,0.143379805101228,3.36492630429559));
#22368=CARTESIAN_POINT('Ctrl Pts',(12.809430733463,0.42764021116234,3.50908227080648));
#22369=CARTESIAN_POINT('Ctrl Pts',(12.8330448496128,0.609413666055986,3.77089008898231));
#22370=CARTESIAN_POINT('Ctrl Pts',(12.8566589657627,0.645136892431096,4.08760569204938));
#22371=CARTESIAN_POINT('Ctrl Pts',(12.8802730819125,0.526248572038732,4.38332598125533));
#22372=CARTESIAN_POINT('Ctrl Pts',(12.903124993225,0.289149347937084,4.5805996458561));
#22373=CARTESIAN_POINT('Ctrl Pts',(12.9181055324875,0.0930307802739178,
4.62497206165088));
#22374=CARTESIAN_POINT('Ctrl Pts',(12.9252146997001,-9.42225863212465E-6,
4.62504029123832));
#22375=CARTESIAN_POINT('Ctrl Pts',(12.5247853002999,3.80998376856706E-6,
4.62503871776264));
#22376=CARTESIAN_POINT('Ctrl Pts',(12.5322662776332,-0.0978890574527522,
4.62500203345524));
#22377=CARTESIAN_POINT('Ctrl Pts',(12.5476186270164,-0.298862923743373,
4.57698368148067));
#22378=CARTESIAN_POINT('Ctrl Pts',(12.5708423484496,-0.535054221536356,
4.37092866956447));
#22379=CARTESIAN_POINT('Ctrl Pts',(12.5944564645995,-0.647009713430093,
4.07251155115386));
#22380=CARTESIAN_POINT('Ctrl Pts',(12.6180705807493,-0.603894380709874,
3.75671714932517));
#22381=CARTESIAN_POINT('Ctrl Pts',(12.6416846968992,-0.416056506175611,
3.49922677321964));
#22382=CARTESIAN_POINT('Ctrl Pts',(12.6652988130491,-0.128505496873939,
3.36175035317655));
#22383=CARTESIAN_POINT('Ctrl Pts',(12.6889129291989,0.189841674427298,3.37723482234205));
#22384=CARTESIAN_POINT('Ctrl Pts',(12.7125270453488,0.462692468193658,3.54196933898577));
#22385=CARTESIAN_POINT('Ctrl Pts',(12.7361411614987,0.624655556881011,3.81647407445394));
#22386=CARTESIAN_POINT('Ctrl Pts',(12.7597552776485,0.636915702199809,4.13496208375113));
#22387=CARTESIAN_POINT('Ctrl Pts',(12.7833693937984,0.496534514683115,4.42110548633398));
#22388=CARTESIAN_POINT('Ctrl Pts',(12.8050460680155,0.258436396781676,4.5911312751119));
#22389=CARTESIAN_POINT('Ctrl Pts',(12.8188513701827,0.0776597756952025,
4.62491945378327));
#22390=CARTESIAN_POINT('Ctrl Pts',(12.8247853002999,-1.55438223423052E-5,
4.62499607812274));
#22391=CARTESIAN_POINT('Ctrl Pts',(12.5,-0.186196943290592,3.58169363627332));
#22392=CARTESIAN_POINT('Ctrl Pts',(12.50787137205,-0.117235947257613,3.55099764935784));
#22393=CARTESIAN_POINT('Ctrl Pts',(12.5236141161499,0.0360970477778841,
3.52440632583991));
#22394=CARTESIAN_POINT('Ctrl Pts',(12.5472282322997,0.257537368848111,3.59853698535937));
#22395=CARTESIAN_POINT('Ctrl Pts',(12.5708423484496,0.417223782598737,3.76887858727216));
#22396=CARTESIAN_POINT('Ctrl Pts',(12.5944564645995,0.476936352215019,3.99461366516243));
#22397=CARTESIAN_POINT('Ctrl Pts',(12.6180705807493,0.422340246895018,4.22163841384584));
#22398=CARTESIAN_POINT('Ctrl Pts',(12.6416846968992,0.266530936180377,4.39554662614981));
#22399=CARTESIAN_POINT('Ctrl Pts',(12.6652988130491,0.0468439715927196,
4.47465904879863));
#22400=CARTESIAN_POINT('Ctrl Pts',(12.6889129291989,-0.184068700558194,
4.44001626345752));
#22401=CARTESIAN_POINT('Ctrl Pts',(12.7125270453488,-0.37086838928987,4.29992045400434));
#22402=CARTESIAN_POINT('Ctrl Pts',(12.7361411614987,-0.468786717745582,
4.08794664964497));
#22403=CARTESIAN_POINT('Ctrl Pts',(12.7597552776485,-0.454357124800734,
3.85489580461101));
#22404=CARTESIAN_POINT('Ctrl Pts',(12.7833693937984,-0.331037647139153,
3.65662019659523));
#22405=CARTESIAN_POINT('Ctrl Pts',(12.8069835099483,-0.128382710063344,
3.54063794582746));
#22406=CARTESIAN_POINT('Ctrl Pts',(12.8305976260981,0.10504004521716,3.53474501052695));
#22407=CARTESIAN_POINT('Ctrl Pts',(12.854211742248,0.31328921869753,3.64035367159283));
#22408=CARTESIAN_POINT('Ctrl Pts',(12.8778258583979,0.446456451752615,3.83215407918844));
#22409=CARTESIAN_POINT('Ctrl Pts',(12.9014399745477,0.47262728739502,4.06417992999538));
#22410=CARTESIAN_POINT('Ctrl Pts',(12.9250540906976,0.385529703875575,4.28082461386765));
#22411=CARTESIAN_POINT('Ctrl Pts',(12.9486682068475,0.206037242841946,4.43016772408018));
#22412=CARTESIAN_POINT('Ctrl Pts',(12.9722823229973,-0.0228334776507366,
4.47641814468844));
#22413=CARTESIAN_POINT('Ctrl Pts',(12.9958964391472,-0.24623199631158,4.40849164040747));
#22414=CARTESIAN_POINT('Ctrl Pts',(13.0195105552971,-0.410619302934066,
4.24266727085754));
#22415=CARTESIAN_POINT('Ctrl Pts',(13.0431246714469,-0.476598835156983,
4.01868600055616));
#22416=CARTESIAN_POINT('Ctrl Pts',(13.0667387875968,-0.428358138764893,
3.79022650014263));
#22417=CARTESIAN_POINT('Ctrl Pts',(13.0903529037467,-0.277458432473742,
3.61204067927388));
#22418=CARTESIAN_POINT('Ctrl Pts',(13.1139670198965,-0.060063881357403,
3.52683201033335));
#22419=CARTESIAN_POINT('Ctrl Pts',(13.1375811360464,0.171725397050831,3.55502134399878));
#22420=CARTESIAN_POINT('Ctrl Pts',(13.1611952521963,0.362359488617447,3.68985291022187));
#22421=CARTESIAN_POINT('Ctrl Pts',(13.1848093683461,0.466151606229838,3.89901338554908));
#22422=CARTESIAN_POINT('Ctrl Pts',(13.208423484496,0.458227246370285,4.13237600603144));
#22423=CARTESIAN_POINT('Ctrl Pts',(13.2320376006459,0.34048553704322,4.3340137951542));
#22424=CARTESIAN_POINT('Ctrl Pts',(13.2556517167957,0.141144098528766,4.45560285308526));
#22425=CARTESIAN_POINT('Ctrl Pts',(13.2792658329456,-0.0920235057499227,
4.46800351566886));
#22426=CARTESIAN_POINT('Ctrl Pts',(13.3028799490955,-0.30313703626889,4.36824387779166));
#22427=CARTESIAN_POINT('Ctrl Pts',(13.3264940652453,-0.441601665806575,
4.18023203113149));
#22428=CARTESIAN_POINT('Ctrl Pts',(13.3501081813952,-0.47423338199515,3.94902632355453));
#22429=CARTESIAN_POINT('Ctrl Pts',(13.3737222975451,-0.393211766889608,
3.73003681238273));
#22430=CARTESIAN_POINT('Ctrl Pts',(13.3973364136949,-0.217954214568861,
3.57574585842847));
#22431=CARTESIAN_POINT('Ctrl Pts',(13.4209505298448,0.00953758252632317,
3.52313036287841));
#22432=CARTESIAN_POINT('Ctrl Pts',(13.4445646459947,0.234743631574736,3.58479999551538));
#22433=CARTESIAN_POINT('Ctrl Pts',(13.4681787621445,0.403691735186444,3.74597519957476));
#22434=CARTESIAN_POINT('Ctrl Pts',(13.4917928782944,0.475892304226004,3.96802921540861));
#22435=CARTESIAN_POINT('Ctrl Pts',(13.5154069944443,0.434041969710506,4.19774525232923));
#22436=CARTESIAN_POINT('Ctrl Pts',(13.5390211105941,0.288170455640921,4.38007026295756));
#22437=CARTESIAN_POINT('Ctrl Pts',(13.562635226744,0.0732368858249759,4.47130878927046));
#22438=CARTESIAN_POINT('Ctrl Pts',(13.5862493428939,-0.159248413505658,
4.44959488329479));
#22439=CARTESIAN_POINT('Ctrl Pts',(13.6098634590437,-0.353568721957589,
4.32013243375547));
#22440=CARTESIAN_POINT('Ctrl Pts',(13.6334775751936,-0.46315382488092,4.1139480179165));
#22441=CARTESIAN_POINT('Ctrl Pts',(13.6570916913435,-0.461740889501104,
3.88045516635315));
#22442=CARTESIAN_POINT('Ctrl Pts',(13.6807058074933,-0.349668535617837,
3.67561206636528));
#22443=CARTESIAN_POINT('Ctrl Pts',(13.7043199236432,-0.153795683012805,
3.5485107928471));
#22444=CARTESIAN_POINT('Ctrl Pts',(13.7279340397931,0.0789353756500159,
3.5296120507922));
#22445=CARTESIAN_POINT('Ctrl Pts',(13.7515481559429,0.292749022042461,3.62344505529457));
#22446=CARTESIAN_POINT('Ctrl Pts',(13.7751622720928,0.436403327377467,3.80752207362193));
#22447=CARTESIAN_POINT('Ctrl Pts',(13.7987763882427,0.475470537355291,4.03772776690975));
#22448=CARTESIAN_POINT('Ctrl Pts',(13.8223905043925,0.400587923144683,4.25889173822189));
#22449=CARTESIAN_POINT('Ctrl Pts',(13.8460046205424,0.229701624524423,4.41801050223621));
#22450=CARTESIAN_POINT('Ctrl Pts',(13.8696187366923,0.00376573255618155,
4.47695013947711));
#22451=CARTESIAN_POINT('Ctrl Pts',(13.8932328528421,-0.223072643433687,
4.42158535558109));
#22452=CARTESIAN_POINT('Ctrl Pts',(13.916846968992,-0.396450107540549,4.26518470642179));
#22453=CARTESIAN_POINT('Ctrl Pts',(13.9404610851419,-0.474815543552022,
4.04523069632808));
#22454=CARTESIAN_POINT('Ctrl Pts',(13.9640752012917,-0.439388129199652,
3.81443683499316));
#22455=CARTESIAN_POINT('Ctrl Pts',(13.9876893174416,-0.298658290955197,
3.62811447792009));
#22456=CARTESIAN_POINT('Ctrl Pts',(14.0113034335915,-0.0863529142219465,
3.53091707503438));
#22457=CARTESIAN_POINT('Ctrl Pts',(14.0349175497413,0.146647539536438,3.54613866056158));
#22458=CARTESIAN_POINT('Ctrl Pts',(14.0585316658912,0.344502889581789,3.6701312755675));
#22459=CARTESIAN_POINT('Ctrl Pts',(14.0821457820411,0.459795723937725,3.87317922671144));
#22460=CARTESIAN_POINT('Ctrl Pts',(14.1057598981909,0.464895312258427,4.10662065901627));
#22461=CARTESIAN_POINT('Ctrl Pts',(14.1293740143408,0.358579502702881,4.31450970816539));
#22462=CARTESIAN_POINT('Ctrl Pts',(14.1529881304907,0.166327619131383,4.44702431634421));
#22463=CARTESIAN_POINT('Ctrl Pts',(14.1766022466405,-0.0657858362277661,
4.47240643522367));
#22464=CARTESIAN_POINT('Ctrl Pts',(14.2002163627904,-0.282133257977474,
4.38457306332079));
#22465=CARTESIAN_POINT('Ctrl Pts',(14.2238304789403,-0.430865480427841,
4.20457407964992));
#22466=CARTESIAN_POINT('Ctrl Pts',(14.2474445950901,-0.476337791093329,
3.97554749368157));
#22467=CARTESIAN_POINT('Ctrl Pts',(14.27105871124,-0.407652434174819,3.75238112107461));
#22468=CARTESIAN_POINT('Ctrl Pts',(14.2946728273899,-0.241270333599833,
3.58855833656088));
#22469=CARTESIAN_POINT('Ctrl Pts',(14.3182869435397,-0.0170661180132474,
3.52334041087493));
#22470=CARTESIAN_POINT('Ctrl Pts',(14.3419010596896,0.211228111558234,3.57235727391142));
#22471=CARTESIAN_POINT('Ctrl Pts',(14.3655151758395,0.388900053764453,3.72386169322071));
#22472=CARTESIAN_POINT('Ctrl Pts',(14.3891292919893,0.473369390821204,3.94154458004181));
#22473=CARTESIAN_POINT('Ctrl Pts',(14.4127434081392,0.444392458083208,4.17323671518384));
#22474=CARTESIAN_POINT('Ctrl Pts',(14.4363575242891,0.308913779199362,4.3634114655727));
#22475=CARTESIAN_POINT('Ctrl Pts',(14.4599716404389,0.0994017626770733,
4.46649212840691));
#22476=CARTESIAN_POINT('Ctrl Pts',(14.4835857565888,-0.133932578240045,
4.45777470525894));
#22477=CARTESIAN_POINT('Ctrl Pts',(14.5071998727387,-0.335169044432007,
4.33934838727104));
#22478=CARTESIAN_POINT('Ctrl Pts',(14.5308139888885,-0.456079915900645,
4.13959486595487));
#22479=CARTESIAN_POINT('Ctrl Pts',(14.5544281050384,-0.467688060597361,
3.90638646324521));
#22480=CARTESIAN_POINT('Ctrl Pts',(14.5780422211883,-0.367211505836647,
3.69561319629505));
#22481=CARTESIAN_POINT('Ctrl Pts',(14.6016563373381,-0.178730157419731,
3.55778834579073));
#22482=CARTESIAN_POINT('Ctrl Pts',(14.625270453488,0.0525851174261518,3.52594259660587));
#22483=CARTESIAN_POINT('Ctrl Pts',(14.6488845696379,0.271298002813252,3.60770800421126));
#22484=CARTESIAN_POINT('Ctrl Pts',(14.6724986857877,0.424992433239313,3.78348891949988));
#22485=CARTESIAN_POINT('Ctrl Pts',(14.6961128019376,0.476834468501385,4.01115822240469));
#22486=CARTESIAN_POINT('Ctrl Pts',(14.7197269180875,0.414399804028447,4.23615337970372));
#22487=CARTESIAN_POINT('Ctrl Pts',(14.7433410342373,0.252651341641402,4.40455273546398));
#22488=CARTESIAN_POINT('Ctrl Pts',(14.7669551503872,0.0303532266559796,
4.47599821226155));
#22489=CARTESIAN_POINT('Ctrl Pts',(14.7905692665371,-0.199219250862459,
4.43336740322118));
#22490=CARTESIAN_POINT('Ctrl Pts',(14.8141833826869,-0.381047447081096,
4.28687708064914));
#22491=CARTESIAN_POINT('Ctrl Pts',(14.8377974988368,-0.471554972144783,
4.07163466550741));
#22492=CARTESIAN_POINT('Ctrl Pts',(14.8614116149867,-0.449051060899263,
3.83922451083896));
#22493=CARTESIAN_POINT('Ctrl Pts',(14.8850257311365,-0.318928946727196,
3.64534530693059));
#22494=CARTESIAN_POINT('Ctrl Pts',(14.9086398472864,-0.112373269271187,
3.53646160000302));
#22495=CARTESIAN_POINT('Ctrl Pts',(14.9322539634362,0.121113399391719,3.5386680312482));
#22496=CARTESIAN_POINT('Ctrl Pts',(14.9558680795861,0.325574495333277,3.65143602219853));
#22497=CARTESIAN_POINT('Ctrl Pts',(14.979482195736,0.452009190454857,3.84773949289016));
#22498=CARTESIAN_POINT('Ctrl Pts',(15.0030963118858,0.470117180575255,4.08053390545391));
#22499=CARTESIAN_POINT('Ctrl Pts',(15.0267104280357,0.375557372208547,4.29402641177155));
#22500=CARTESIAN_POINT('Ctrl Pts',(15.0503245441856,0.190994688421392,4.43705643304037));
#22501=CARTESIAN_POINT('Ctrl Pts',(15.0739386603355,-0.0393454023191647,
4.47533644032795));
#22502=CARTESIAN_POINT('Ctrl Pts',(15.0975527764853,-0.260245916509526,
4.39971253597763));
#22503=CARTESIAN_POINT('Ctrl Pts',(15.1211668926352,-0.418792603204267,
4.22826540530875));
#22504=CARTESIAN_POINT('Ctrl Pts',(15.1369096367351,-0.457530945318996,
4.07754232577813));
#22505=CARTESIAN_POINT('Ctrl Pts',(15.1447810087851,-0.457870370902723,
4.00205890126089));
#22506=CARTESIAN_POINT('Ctrl Pts',(12.4850729970717,-0.208850989443975,
3.53079950502365));
#22507=CARTESIAN_POINT('Ctrl Pts',(12.4929443691216,-0.131499707516366,
3.49636882573344));
#22508=CARTESIAN_POINT('Ctrl Pts',(12.5086871132215,0.0404888716816997,
3.46654221242176));
#22509=CARTESIAN_POINT('Ctrl Pts',(12.5323012293714,0.288871199237585,3.54969213591223));
#22510=CARTESIAN_POINT('Ctrl Pts',(12.5559153455212,0.467986199318594,3.74075871022993));
#22511=CARTESIAN_POINT('Ctrl Pts',(12.5795294616711,0.534963825407437,3.99395832530641));
#22512=CARTESIAN_POINT('Ctrl Pts',(12.603143577821,0.473725169098917,4.24860452170932));
#22513=CARTESIAN_POINT('Ctrl Pts',(12.6267576939708,0.298958988020687,4.4436716456386));
#22514=CARTESIAN_POINT('Ctrl Pts',(12.6503718101207,0.0525433427838623,
4.53240944903922));
#22515=CARTESIAN_POINT('Ctrl Pts',(12.6739859262706,-0.206463809544117,
4.49355177571912));
#22516=CARTESIAN_POINT('Ctrl Pts',(12.6976000424205,-0.41599087873209,4.33641091237214));
#22517=CARTESIAN_POINT('Ctrl Pts',(12.7212141585703,-0.525822648369464,
4.09864686536754));
#22518=CARTESIAN_POINT('Ctrl Pts',(12.7448282747202,-0.509637448384189,
3.8372413948162));
#22519=CARTESIAN_POINT('Ctrl Pts',(12.76844239087,-0.37131404483003,3.61484216427635));
#22520=CARTESIAN_POINT('Ctrl Pts',(12.7920565070199,-0.144002664868576,
3.48474868689319));
#22521=CARTESIAN_POINT('Ctrl Pts',(12.8156706231698,0.117819965178516,3.47813877511649));
#22522=CARTESIAN_POINT('Ctrl Pts',(12.8392847393197,0.351406216185799,3.59659653799738));
#22523=CARTESIAN_POINT('Ctrl Pts',(12.8628988554695,0.500775523187073,3.81173274911973));
#22524=CARTESIAN_POINT('Ctrl Pts',(12.8865129716194,0.530130489073712,4.07198851734671));
#22525=CARTESIAN_POINT('Ctrl Pts',(12.9101270877692,0.432435993263294,4.31499173633021));
#22526=CARTESIAN_POINT('Ctrl Pts',(12.9337412039191,0.231105201134755,4.48250499290311));
#22527=CARTESIAN_POINT('Ctrl Pts',(12.957355320069,-0.0256115611541523,
4.53438256906268));
#22528=CARTESIAN_POINT('Ctrl Pts',(12.9809694362189,-0.276190334565159,
4.45819164252092));
#22529=CARTESIAN_POINT('Ctrl Pts',(13.0045835523687,-0.460578171623014,
4.27219189922559));
#22530=CARTESIAN_POINT('Ctrl Pts',(13.0281976685186,-0.534585243620437,
4.0209594724593));
#22531=CARTESIAN_POINT('Ctrl Pts',(13.0518117846684,-0.480475240551103,
3.76470396221295));
#22532=CARTESIAN_POINT('Ctrl Pts',(13.0754259008183,-0.311216001335094,
3.5648387853972));
#22533=CARTESIAN_POINT('Ctrl Pts',(13.0990400169682,-0.0673716809183137,
3.46926302296559));
#22534=CARTESIAN_POINT('Ctrl Pts',(13.122654133118,0.19261873182715,3.50088207171981));
#22535=CARTESIAN_POINT('Ctrl Pts',(13.1462682492679,0.406446724606302,3.65211820651514));
#22536=CARTESIAN_POINT('Ctrl Pts',(13.1698823654178,0.522866930420328,3.88672663484193));
#22537=CARTESIAN_POINT('Ctrl Pts',(13.1934964815676,0.513978436505609,4.14848181366307));
#22538=CARTESIAN_POINT('Ctrl Pts',(13.2171105977175,0.381911432304553,4.37465229220773));
#22539=CARTESIAN_POINT('Ctrl Pts',(13.2407247138674,0.158316694737061,4.51103474084347));
#22540=CARTESIAN_POINT('Ctrl Pts',(13.2643388300172,-0.103219740820234,
4.52494415635039));
#22541=CARTESIAN_POINT('Ctrl Pts',(13.2879529461671,-0.340018846942428,
4.41304705047411));
#22542=CARTESIAN_POINT('Ctrl Pts',(13.311567062317,-0.495330069408668,4.20216034359148));
#22543=CARTESIAN_POINT('Ctrl Pts',(13.3351811784669,-0.531931992580964,
3.94282450306062));
#22544=CARTESIAN_POINT('Ctrl Pts',(13.3587952946167,-0.44105271077271,3.69719116838925));
#22545=CARTESIAN_POINT('Ctrl Pts',(13.3824094107666,-0.244472076510672,
3.5241280781681));
#22546=CARTESIAN_POINT('Ctrl Pts',(13.4060235269164,0.0106979927399635,
3.46511100671938));
#22547=CARTESIAN_POINT('Ctrl Pts',(13.4296376430663,0.263304213558122,3.53428380605355));
#22548=CARTESIAN_POINT('Ctrl Pts',(13.4532517592162,0.452807746647384,3.71506873327496));
#22549=CARTESIAN_POINT('Ctrl Pts',(13.476865875366,0.533792751104717,3.96413942206993));
#22550=CARTESIAN_POINT('Ctrl Pts',(13.5004799915159,0.486850606847911,4.22180434800346));
#22551=CARTESIAN_POINT('Ctrl Pts',(13.5240941076658,0.323231325528255,4.42631231788287));
#22552=CARTESIAN_POINT('Ctrl Pts',(13.5477082238157,0.0821474069231642,
4.52865157307741));
#22553=CARTESIAN_POINT('Ctrl Pts',(13.5713223399655,-0.178623709606947,
4.50429579866153));
#22554=CARTESIAN_POINT('Ctrl Pts',(13.5949364561154,-0.396586410669692,
4.35908202552279));
#22555=CARTESIAN_POINT('Ctrl Pts',(13.6185505722652,-0.519504417643299,
4.12781174527607));
#22556=CARTESIAN_POINT('Ctrl Pts',(13.6421646884151,-0.517919574482721,
3.86591049053316));
#22557=CARTESIAN_POINT('Ctrl Pts',(13.665778804565,-0.392211699884016,3.6361447201764));
#22558=CARTESIAN_POINT('Ctrl Pts',(13.6893929207148,-0.172507561089802,
3.49357940054904));
#22559=CARTESIAN_POINT('Ctrl Pts',(13.7130070368647,0.0885392156030666,
3.47238130294519));
#22560=CARTESIAN_POINT('Ctrl Pts',(13.7366211530146,0.328366952925232,3.57763069902274));
#22561=CARTESIAN_POINT('Ctrl Pts',(13.7602352691644,0.489499264105438,3.78410383833506));
#22562=CARTESIAN_POINT('Ctrl Pts',(13.7838493853143,0.533319669072828,4.04231799571659));
#22563=CARTESIAN_POINT('Ctrl Pts',(13.8074635014642,0.449326302728307,4.29039035083475));
#22564=CARTESIAN_POINT('Ctrl Pts',(13.831077617614,0.257648760022572,4.46886863686992));
#22565=CARTESIAN_POINT('Ctrl Pts',(13.8546917337639,0.00422389839726028,
4.53497929012603));
#22566=CARTESIAN_POINT('Ctrl Pts',(13.8783058499138,-0.25021324988294,4.47287843233165));
#22567=CARTESIAN_POINT('Ctrl Pts',(13.9019199660636,-0.444685051009628,
4.29744896636227));
#22568=CARTESIAN_POINT('Ctrl Pts',(13.9255340822135,-0.532584984058807,
4.05073378496132));
#22569=CARTESIAN_POINT('Ctrl Pts',(13.9491481983634,-0.492847218174075,
3.79185989881933));
#22570=CARTESIAN_POINT('Ctrl Pts',(13.9727623145132,-0.334995185577738,
3.58286823685896));
#22571=CARTESIAN_POINT('Ctrl Pts',(13.9963764306631,-0.0968592247428986,
3.47384510573062));
#22572=CARTESIAN_POINT('Ctrl Pts',(14.019990546813,0.164489723571401,3.49091865775613));
#22573=CARTESIAN_POINT('Ctrl Pts',(14.0436046629628,0.386417564563212,3.62999709733779));
#22574=CARTESIAN_POINT('Ctrl Pts',(14.0672187791127,0.515737746224078,3.85774930825782));
#22575=CARTESIAN_POINT('Ctrl Pts',(14.0908328952626,0.521457786777448,4.11959288770904));
#22576=CARTESIAN_POINT('Ctrl Pts',(14.1144470114124,0.402206838685568,4.35277519909424));
#22577=CARTESIAN_POINT('Ctrl Pts',(14.1380611275623,0.186564221804844,4.50141247822903));
#22578=CARTESIAN_POINT('Ctrl Pts',(14.1616752437122,-0.0737898095680628,
4.52988276645436));
#22579=CARTESIAN_POINT('Ctrl Pts',(14.185289359862,-0.316459599402161,4.43136296100575));
#22580=CARTESIAN_POINT('Ctrl Pts',(14.2089034760119,-0.483287643257218,
4.22946401908862));
#22581=CARTESIAN_POINT('Ctrl Pts',(14.2325175921618,-0.53429243907693,3.97257242762026));
#22582=CARTESIAN_POINT('Ctrl Pts',(14.2561317083116,-0.457250332481466,
3.72225404480531));
#22583=CARTESIAN_POINT('Ctrl Pts',(14.2797458244615,-0.270625000632592,
3.53849941363631));
#22584=CARTESIAN_POINT('Ctrl Pts',(14.3033599406114,-0.0191425034699505,
3.46534661065105));
#22585=CARTESIAN_POINT('Ctrl Pts',(14.3269740567612,0.236927627906706,3.52032721432634));
#22586=CARTESIAN_POINT('Ctrl Pts',(14.3505881729111,0.436216403922163,3.69026474025285));
#22587=CARTESIAN_POINT('Ctrl Pts',(14.374202289061,0.530962882087739,3.93443247734966));
#22588=CARTESIAN_POINT('Ctrl Pts',(14.3978164052108,0.498460409348769,4.19431392768733));
#22589=CARTESIAN_POINT('Ctrl Pts',(14.4214305213607,0.346498429557861,4.40762669256976));
#22590=CARTESIAN_POINT('Ctrl Pts',(14.4450446375106,0.111495689030631,4.52324888295055));
#22591=CARTESIAN_POINT('Ctrl Pts',(14.4686587536604,-0.150227769531968,
4.51347083601981));
#22592=CARTESIAN_POINT('Ctrl Pts',(14.4922728698103,-0.375948097339969,
4.38063592879268));
#22593=CARTESIAN_POINT('Ctrl Pts',(14.5158869859602,-0.51156984651846,4.15657897149511));
#22594=CARTESIAN_POINT('Ctrl Pts',(14.53950110211,-0.52459032076832,3.89499677367918));
#22595=CARTESIAN_POINT('Ctrl Pts',(14.5631152182599,-0.411889072794842,
3.65857933001481));
#22596=CARTESIAN_POINT('Ctrl Pts',(14.5867293344098,-0.200475741228102,
3.50398572665543));
#22597=CARTESIAN_POINT('Ctrl Pts',(14.6103434505596,0.0589829973059192,
3.46826539682992));
#22598=CARTESIAN_POINT('Ctrl Pts',(14.6339575667095,0.304306049929579,3.5599789662306));
#22599=CARTESIAN_POINT('Ctrl Pts',(14.6575716828594,0.476700039321847,3.75714663952638));
#22600=CARTESIAN_POINT('Ctrl Pts',(14.6811857990092,0.53484954579562,4.0125158112076));
#22601=CARTESIAN_POINT('Ctrl Pts',(14.7047999151591,0.464818635404008,4.26488548168423));
#22602=CARTESIAN_POINT('Ctrl Pts',(14.728414031309,0.283390703164248,4.45377350235044));
#22603=CARTESIAN_POINT('Ctrl Pts',(14.7520281474588,0.0340462163765225,
4.5339115446661));
#22604=CARTESIAN_POINT('Ctrl Pts',(14.7756422636087,-0.223457683695575,
4.48609396779546));
#22605=CARTESIAN_POINT('Ctrl Pts',(14.7992563797586,-0.427408393186059,
4.32178058932398));
#22606=CARTESIAN_POINT('Ctrl Pts',(14.8228704959084,-0.528927708313459,
4.08035024907128));
#22607=CARTESIAN_POINT('Ctrl Pts',(14.8464846120583,-0.503685810960444,
3.81966341983811));
#22608=CARTESIAN_POINT('Ctrl Pts',(14.8700987282082,-0.357732113691821,
3.6021954912391));
#22609=CARTESIAN_POINT('Ctrl Pts',(14.893712844358,-0.126045401495737,3.48006421709321));
#22610=CARTESIAN_POINT('Ctrl Pts',(14.9173269605079,0.13584891809103,3.48253909847714));
#22611=CARTESIAN_POINT('Ctrl Pts',(14.9409410766578,0.365186207068703,3.60902724630258));
#22612=CARTESIAN_POINT('Ctrl Pts',(14.9645551928076,0.507003847624586,3.82921439524653));
#22613=CARTESIAN_POINT('Ctrl Pts',(14.9881693089575,0.52731498478211,4.0903322339271));
#22614=CARTESIAN_POINT('Ctrl Pts',(15.0117834251074,0.421250356706029,4.32979975898591));
#22615=CARTESIAN_POINT('Ctrl Pts',(15.0353975412572,0.214232462415332,4.49023183125449));
#22616=CARTESIAN_POINT('Ctrl Pts',(15.0590116574071,-0.0441324441701724,
4.53316925684615));
#22617=CARTESIAN_POINT('Ctrl Pts',(15.082625773557,-0.291909288096862,4.4483444097243));
#22618=CARTESIAN_POINT('Ctrl Pts',(15.1062398897068,-0.469745893811612,
4.25603780014884));
#22619=CARTESIAN_POINT('Ctrl Pts',(15.1219826338067,-0.513197418509596,
4.08697667736293));
#22620=CARTESIAN_POINT('Ctrl Pts',(15.1298540058567,-0.513578141027115,
4.0023094018511));
#22621=CARTESIAN_POINT('Ctrl Pts',(12.4701459941433,-0.231505035597357,
3.47990537377399));
#22622=CARTESIAN_POINT('Ctrl Pts',(12.4780173661933,-0.145763467775118,
3.44174000210903));
#22623=CARTESIAN_POINT('Ctrl Pts',(12.4937601102932,0.0448806955855158,
3.40867809900361));
#22624=CARTESIAN_POINT('Ctrl Pts',(12.517374226443,0.320205029627059,3.5008472864651));
#22625=CARTESIAN_POINT('Ctrl Pts',(12.5409883425929,0.518748616038451,3.71263883318769));
#22626=CARTESIAN_POINT('Ctrl Pts',(12.5646024587428,0.592991298599855,3.99330298545039));
#22627=CARTESIAN_POINT('Ctrl Pts',(12.5882165748926,0.525110091302815,4.27557062957281));
#22628=CARTESIAN_POINT('Ctrl Pts',(12.6118306910425,0.331387039860997,4.49179666512739));
#22629=CARTESIAN_POINT('Ctrl Pts',(12.6354448071924,0.0582427139750047,
4.5901598492798));
#22630=CARTESIAN_POINT('Ctrl Pts',(12.6590589233422,-0.22885891853004,4.54708728798072));
#22631=CARTESIAN_POINT('Ctrl Pts',(12.6826730394921,-0.461113368174311,
4.37290137073994));
#22632=CARTESIAN_POINT('Ctrl Pts',(12.706287155642,-0.582858578993347,4.10934708109011));
#22633=CARTESIAN_POINT('Ctrl Pts',(12.7299012717918,-0.564917771967644,
3.8195869850214));
#22634=CARTESIAN_POINT('Ctrl Pts',(12.7535153879417,-0.411590442520908,
3.57306413195747));
#22635=CARTESIAN_POINT('Ctrl Pts',(12.7771295040916,-0.159622619673808,
3.42885942795892));
#22636=CARTESIAN_POINT('Ctrl Pts',(12.8007436202414,0.130599885139872,3.42153253970604));
#22637=CARTESIAN_POINT('Ctrl Pts',(12.8243577363913,0.38952321367407,3.55283940440193));
#22638=CARTESIAN_POINT('Ctrl Pts',(12.8479718525412,0.555094594621529,3.79131141905102));
#22639=CARTESIAN_POINT('Ctrl Pts',(12.871585968691,0.587633690752404,4.07979710469805));
#22640=CARTESIAN_POINT('Ctrl Pts',(12.8952000848409,0.479342282651013,4.34915885879276));
#22641=CARTESIAN_POINT('Ctrl Pts',(12.9188142009908,0.256173159427565,4.53484226172604));
#22642=CARTESIAN_POINT('Ctrl Pts',(12.9424283171406,-0.0283896446575681,
4.59234699343691));
#22643=CARTESIAN_POINT('Ctrl Pts',(12.9660424332905,-0.306148672818738,
4.50789164463438));
#22644=CARTESIAN_POINT('Ctrl Pts',(12.9896565494404,-0.510537040311962,
4.30171652759364));
#22645=CARTESIAN_POINT('Ctrl Pts',(13.0132706655902,-0.59257165208389,4.02323294436244));
#22646=CARTESIAN_POINT('Ctrl Pts',(13.0368847817401,-0.532592342337314,
3.73918142428326));
#22647=CARTESIAN_POINT('Ctrl Pts',(13.06049889789,-0.344973570196446,3.51763689152052));
#22648=CARTESIAN_POINT('Ctrl Pts',(13.0841130140398,-0.0746794804792245,
3.41169403559782));
#22649=CARTESIAN_POINT('Ctrl Pts',(13.1077271301897,0.213512066603468,3.44674279944083));
#22650=CARTESIAN_POINT('Ctrl Pts',(13.1313412463396,0.450533960595157,3.6143835028084));
#22651=CARTESIAN_POINT('Ctrl Pts',(13.1549553624894,0.579582254610818,3.87443988413478));
#22652=CARTESIAN_POINT('Ctrl Pts',(13.1785694786393,0.569729626640933,4.1645876212947));
#22653=CARTESIAN_POINT('Ctrl Pts',(13.2021835947892,0.423337327565886,4.41529078926125));
#22654=CARTESIAN_POINT('Ctrl Pts',(13.225797710939,0.175489290945357,4.56646662860168));
#22655=CARTESIAN_POINT('Ctrl Pts',(13.2494118270889,-0.114415975890545,
4.58188479703192));
#22656=CARTESIAN_POINT('Ctrl Pts',(13.2730259432388,-0.376900657615966,
4.45785022315656));
#22657=CARTESIAN_POINT('Ctrl Pts',(13.2966400593886,-0.54905847301076,4.22408865605146));
#22658=CARTESIAN_POINT('Ctrl Pts',(13.3202541755385,-0.589630603166779,
3.93662268256671));
#22659=CARTESIAN_POINT('Ctrl Pts',(13.3438682916884,-0.488893654655812,
3.66434552439578));
#22660=CARTESIAN_POINT('Ctrl Pts',(13.3674824078382,-0.270989938452484,
3.47251029790774));
#22661=CARTESIAN_POINT('Ctrl Pts',(13.3910965239881,0.0118584029536041,
3.40709165056035));
#22662=CARTESIAN_POINT('Ctrl Pts',(13.414710640138,0.291864795541507,3.48376761659174));
#22663=CARTESIAN_POINT('Ctrl Pts',(13.4383247562878,0.501923758108325,3.68416226697515));
#22664=CARTESIAN_POINT('Ctrl Pts',(13.4619388724377,0.591693197983429,3.96024962873126));
#22665=CARTESIAN_POINT('Ctrl Pts',(13.4855529885876,0.539659243985316,4.2458634436777));
#22666=CARTESIAN_POINT('Ctrl Pts',(13.5091671047374,0.358292195415589,4.47255437280819));
#22667=CARTESIAN_POINT('Ctrl Pts',(13.5327812208873,0.0910579280213527,
4.58599435688436));
#22668=CARTESIAN_POINT('Ctrl Pts',(13.5563953370372,-0.197999005708236,
4.55899671402827));
#22669=CARTESIAN_POINT('Ctrl Pts',(13.580009453187,-0.439604099381795,4.39803161729011));
#22670=CARTESIAN_POINT('Ctrl Pts',(13.6036235693369,-0.575855010405679,
4.14167547263565));
#22671=CARTESIAN_POINT('Ctrl Pts',(13.6272376854868,-0.574098259464336,
3.85136581471317));
#22672=CARTESIAN_POINT('Ctrl Pts',(13.6508518016366,-0.434754864150196,
3.59667737398752));
#22673=CARTESIAN_POINT('Ctrl Pts',(13.6744659177865,-0.191219439166798,
3.43864800825098));
#22674=CARTESIAN_POINT('Ctrl Pts',(13.6980800339364,0.0981430555561168,
3.41515055509818));
#22675=CARTESIAN_POINT('Ctrl Pts',(13.7216941500862,0.363984883808003,3.53181634275091));
#22676=CARTESIAN_POINT('Ctrl Pts',(13.7453082662361,0.54259520083341,3.76068560304818));
#22677=CARTESIAN_POINT('Ctrl Pts',(13.768922382386,0.591168800790367,4.04690822452342));
#22678=CARTESIAN_POINT('Ctrl Pts',(13.7925364985358,0.498064682311931,4.32188896344761));
#22679=CARTESIAN_POINT('Ctrl Pts',(13.8161506146857,0.28559589552072,4.51972677150362));
#22680=CARTESIAN_POINT('Ctrl Pts',(13.8397647308356,0.00468206423833927,
4.59300844077494));
#22681=CARTESIAN_POINT('Ctrl Pts',(13.8633788469854,-0.277353856332193,
4.52417150908221));
#22682=CARTESIAN_POINT('Ctrl Pts',(13.8869929631353,-0.492919994478707,
4.32971322630275));
#22683=CARTESIAN_POINT('Ctrl Pts',(13.9106070792852,-0.590354424565592,
4.05623687359455));
#22684=CARTESIAN_POINT('Ctrl Pts',(13.934221195435,-0.546306307148498,3.76928296264551));
#22685=CARTESIAN_POINT('Ctrl Pts',(13.9578353115849,-0.371332080200278,
3.53762199579782));
#22686=CARTESIAN_POINT('Ctrl Pts',(13.9814494277348,-0.107365535263851,
3.41677313642685));
#22687=CARTESIAN_POINT('Ctrl Pts',(14.0050635438846,0.182331907606365,3.43569865495067));
#22688=CARTESIAN_POINT('Ctrl Pts',(14.0286776600345,0.428332239544634,3.58986291910809));
#22689=CARTESIAN_POINT('Ctrl Pts',(14.0522917761844,0.571679768510432,3.8423193898042));
#22690=CARTESIAN_POINT('Ctrl Pts',(14.0759058923342,0.578020261296468,4.1325651164018));
#22691=CARTESIAN_POINT('Ctrl Pts',(14.0995200084841,0.445834174668256,4.39104069002309));
#22692=CARTESIAN_POINT('Ctrl Pts',(14.123134124634,0.206800824478305,4.55580064011384));
#22693=CARTESIAN_POINT('Ctrl Pts',(14.1467482407838,-0.0817937829083601,
4.58735909768505));
#22694=CARTESIAN_POINT('Ctrl Pts',(14.1703623569337,-0.350785940826847,
4.4781528586907));
#22695=CARTESIAN_POINT('Ctrl Pts',(14.1939764730836,-0.535709806086595,
4.25435395852733));
#22696=CARTESIAN_POINT('Ctrl Pts',(14.2175905892334,-0.59224708706053,3.96959736155895));
#22697=CARTESIAN_POINT('Ctrl Pts',(14.2412047053833,-0.506848230788112,
3.69212696853602));
#22698=CARTESIAN_POINT('Ctrl Pts',(14.2648188215332,-0.29997966766535,3.48844049071174));
#22699=CARTESIAN_POINT('Ctrl Pts',(14.288432937683,-0.0212188889266537,
3.40735281042717));
#22700=CARTESIAN_POINT('Ctrl Pts',(14.3120470538329,0.262627144255178,3.46829715474127));
#22701=CARTESIAN_POINT('Ctrl Pts',(14.3356611699828,0.483532754079872,3.65666778728498));
#22702=CARTESIAN_POINT('Ctrl Pts',(14.3592752861326,0.588556373354274,3.9273203746575));
#22703=CARTESIAN_POINT('Ctrl Pts',(14.3828894022825,0.55252836061433,4.21539114019081));
#22704=CARTESIAN_POINT('Ctrl Pts',(14.4065035184324,0.384083079916361,4.45184191956682));
#22705=CARTESIAN_POINT('Ctrl Pts',(14.4301176345822,0.123589615384189,4.58000563749418));
#22706=CARTESIAN_POINT('Ctrl Pts',(14.4537317507321,-0.166522960823891,
4.56916696678068));
#22707=CARTESIAN_POINT('Ctrl Pts',(14.477345866882,-0.416727150247931,4.42192347031433));
#22708=CARTESIAN_POINT('Ctrl Pts',(14.5009599830318,-0.567059777136274,
4.17356307703535));
#22709=CARTESIAN_POINT('Ctrl Pts',(14.5245740991817,-0.58149258093928,3.88360708411314));
#22710=CARTESIAN_POINT('Ctrl Pts',(14.5481882153316,-0.456566639753037,
3.62154546373458));
#22711=CARTESIAN_POINT('Ctrl Pts',(14.5718023314814,-0.222221325036472,
3.45018310752014));
#22712=CARTESIAN_POINT('Ctrl Pts',(14.5954164476313,0.0653808771856868,
3.41058819705396));
#22713=CARTESIAN_POINT('Ctrl Pts',(14.6190305637812,0.337314097045906,3.51224992824993));
#22714=CARTESIAN_POINT('Ctrl Pts',(14.642644679931,0.528407645404381,3.73080435955289));
#22715=CARTESIAN_POINT('Ctrl Pts',(14.6662587960809,0.592864623089856,4.0138734000105));
#22716=CARTESIAN_POINT('Ctrl Pts',(14.6898729122308,0.515237466779568,4.29361758366474));
#22717=CARTESIAN_POINT('Ctrl Pts',(14.7134870283806,0.314130064687094,4.5029942692369));
#22718=CARTESIAN_POINT('Ctrl Pts',(14.7371011445305,0.0377392060970651,
4.59182487707066));
#22719=CARTESIAN_POINT('Ctrl Pts',(14.7607152606804,-0.24769611652869,4.53882053236973));
#22720=CARTESIAN_POINT('Ctrl Pts',(14.7843293768302,-0.47376933929102,4.35668409799883));
#22721=CARTESIAN_POINT('Ctrl Pts',(14.8079434929801,-0.586300444482135,
4.08906583263515));
#22722=CARTESIAN_POINT('Ctrl Pts',(14.83155760913,-0.558320561021625,3.80010232883727));
#22723=CARTESIAN_POINT('Ctrl Pts',(14.8551717252798,-0.396535280656446,
3.55904567554761));
#22724=CARTESIAN_POINT('Ctrl Pts',(14.8787858414297,-0.139717533720287,
3.42366683418339));
#22725=CARTESIAN_POINT('Ctrl Pts',(14.9023999575795,0.150584436790342,3.42641016570609));
#22726=CARTESIAN_POINT('Ctrl Pts',(14.9260140737294,0.404797918804129,3.56661847040663));
#22727=CARTESIAN_POINT('Ctrl Pts',(14.9496281898793,0.561998504794314,3.8106892976029));
#22728=CARTESIAN_POINT('Ctrl Pts',(14.9732423060292,0.584512788988964,4.10013056240029));
#22729=CARTESIAN_POINT('Ctrl Pts',(14.996856422179,0.466943341203511,4.36557310620026));
#22730=CARTESIAN_POINT('Ctrl Pts',(15.0204705383289,0.237470236409271,4.54340722946861));
#22731=CARTESIAN_POINT('Ctrl Pts',(15.0440846544788,-0.0489194860211801,
4.59100207336435));
#22732=CARTESIAN_POINT('Ctrl Pts',(15.0676987706286,-0.323572659684198,
4.49697628347096));
#22733=CARTESIAN_POINT('Ctrl Pts',(15.0913128867785,-0.520699184418956,
4.28381019498893));
#22734=CARTESIAN_POINT('Ctrl Pts',(15.1070556308784,-0.568863891700195,
4.09641102894772));
#22735=CARTESIAN_POINT('Ctrl Pts',(15.1149270029284,-0.569285911151507,
4.00255990244131));
#22736=CARTESIAN_POINT('Ctrl Pts',(12.455218991215,-0.25415908175074,3.42901124252432));
#22737=CARTESIAN_POINT('Ctrl Pts',(12.4630903632649,-0.16002722803387,3.38711117848463));
#22738=CARTESIAN_POINT('Ctrl Pts',(12.4788331073648,0.0492725194893315,
3.35081398558546));
#22739=CARTESIAN_POINT('Ctrl Pts',(12.5024472235147,0.351538860016532,3.45200243701797));
#22740=CARTESIAN_POINT('Ctrl Pts',(12.5260613396645,0.569511032758309,3.68451895614546));
#22741=CARTESIAN_POINT('Ctrl Pts',(12.5496754558144,0.651018771792273,3.99264764559437));
#22742=CARTESIAN_POINT('Ctrl Pts',(12.5732895719643,0.576495013506714,4.3025367374363));
#22743=CARTESIAN_POINT('Ctrl Pts',(12.5969036881141,0.363815091701307,4.53992168461618));
#22744=CARTESIAN_POINT('Ctrl Pts',(12.620517804264,0.0639420851661475,4.64791024952038));
#22745=CARTESIAN_POINT('Ctrl Pts',(12.6441319204139,-0.251254027515963,
4.60062280024232));
#22746=CARTESIAN_POINT('Ctrl Pts',(12.6677460365637,-0.506235857616531,
4.40939182910775));
#22747=CARTESIAN_POINT('Ctrl Pts',(12.6913601527136,-0.639894509617229,
4.12004729681268));
#22748=CARTESIAN_POINT('Ctrl Pts',(12.7149742688635,-0.620198095551099,
3.8019325752266));
#22749=CARTESIAN_POINT('Ctrl Pts',(12.7385883850133,-0.451866840211785,
3.53128609963859));
#22750=CARTESIAN_POINT('Ctrl Pts',(12.7622025011632,-0.17524257447904,3.37297016902465));
#22751=CARTESIAN_POINT('Ctrl Pts',(12.7858166173131,0.143379805101228,3.36492630429559));
#22752=CARTESIAN_POINT('Ctrl Pts',(12.809430733463,0.42764021116234,3.50908227080648));
#22753=CARTESIAN_POINT('Ctrl Pts',(12.8330448496128,0.609413666055986,3.77089008898231));
#22754=CARTESIAN_POINT('Ctrl Pts',(12.8566589657627,0.645136892431096,4.08760569204938));
#22755=CARTESIAN_POINT('Ctrl Pts',(12.8802730819125,0.526248572038732,4.38332598125533));
#22756=CARTESIAN_POINT('Ctrl Pts',(12.9038871980624,0.281241117720374,4.58717953054897));
#22757=CARTESIAN_POINT('Ctrl Pts',(12.9275013142123,-0.0311677281609838,
4.65031141781114));
#22758=CARTESIAN_POINT('Ctrl Pts',(12.9511154303622,-0.336107011072318,
4.55759164674784));
#22759=CARTESIAN_POINT('Ctrl Pts',(12.974729546512,-0.56049590900091,4.33124115596169));
#22760=CARTESIAN_POINT('Ctrl Pts',(12.9983436626619,-0.650558060547343,
4.02550641626558));
#22761=CARTESIAN_POINT('Ctrl Pts',(13.0219577788117,-0.584709444123524,
3.71365888635357));
#22762=CARTESIAN_POINT('Ctrl Pts',(13.0455718949616,-0.378731139057797,
3.47043499764384));
#22763=CARTESIAN_POINT('Ctrl Pts',(13.0691860111115,-0.0819872800401352,
3.35412504823007));
#22764=CARTESIAN_POINT('Ctrl Pts',(13.0928001272613,0.234405401379786,3.39260352716186));
#22765=CARTESIAN_POINT('Ctrl Pts',(13.1164142434112,0.494621196584012,3.57664879910166));
#22766=CARTESIAN_POINT('Ctrl Pts',(13.1400283595611,0.636297578801308,3.86215313342763));
#22767=CARTESIAN_POINT('Ctrl Pts',(13.1636424757109,0.625480816776257,4.18069342892634));
#22768=CARTESIAN_POINT('Ctrl Pts',(13.1872565918608,0.464763222827219,4.45592928631477));
#22769=CARTESIAN_POINT('Ctrl Pts',(13.2108707080107,0.192661887153653,4.62189851635989));
#22770=CARTESIAN_POINT('Ctrl Pts',(13.2344848241605,-0.125612210960856,
4.63882543771344));
#22771=CARTESIAN_POINT('Ctrl Pts',(13.2580989403104,-0.413782468289504,
4.50265339583901));
#22772=CARTESIAN_POINT('Ctrl Pts',(13.2817130564603,-0.602786876612853,
4.24601696851145));
#22773=CARTESIAN_POINT('Ctrl Pts',(13.3053271726101,-0.647329213752593,
3.9304208620728));
#22774=CARTESIAN_POINT('Ctrl Pts',(13.32894128876,-0.536734598538914,3.6314998804023));
#22775=CARTESIAN_POINT('Ctrl Pts',(13.3525554049099,-0.297507800394296,
3.42089251764738));
#22776=CARTESIAN_POINT('Ctrl Pts',(13.3761695210598,0.0130188131672444,
3.34907229440132));
#22777=CARTESIAN_POINT('Ctrl Pts',(13.3997836372096,0.320425377524893,3.43325142712992));
#22778=CARTESIAN_POINT('Ctrl Pts',(13.4233977533595,0.551039769569266,3.65325580067535));
#22779=CARTESIAN_POINT('Ctrl Pts',(13.4470118695093,0.649593644862141,3.95635983539258));
#22780=CARTESIAN_POINT('Ctrl Pts',(13.4706259856592,0.592467881122722,4.26992253935193));
#22781=CARTESIAN_POINT('Ctrl Pts',(13.4942401018091,0.393353065302923,4.5187964277335));
#22782=CARTESIAN_POINT('Ctrl Pts',(13.5178542179589,0.0999684491195412,
4.64333714069132));
#22783=CARTESIAN_POINT('Ctrl Pts',(13.5414683341088,-0.217374301809525,
4.61369762939502));
#22784=CARTESIAN_POINT('Ctrl Pts',(13.5650824502587,-0.482621788093898,
4.43698120905743));
#22785=CARTESIAN_POINT('Ctrl Pts',(13.5886965664085,-0.632205603168059,
4.15553919999523));
#22786=CARTESIAN_POINT('Ctrl Pts',(13.6123106825584,-0.630276944445953,
3.83682113889318));
#22787=CARTESIAN_POINT('Ctrl Pts',(13.6359247987083,-0.477298028416376,
3.55721002779864));
#22788=CARTESIAN_POINT('Ctrl Pts',(13.6595389148582,-0.209931317243796,
3.38371661595291));
#22789=CARTESIAN_POINT('Ctrl Pts',(13.683153031008,0.107746895509167,3.35791980725116));
#22790=CARTESIAN_POINT('Ctrl Pts',(13.7067671471579,0.399602814690774,3.48600198647908));
#22791=CARTESIAN_POINT('Ctrl Pts',(13.7303812633077,0.59569113756138,3.73726736776131));
#22792=CARTESIAN_POINT('Ctrl Pts',(13.7539953794576,0.649017932507905,4.05149845333026));
#22793=CARTESIAN_POINT('Ctrl Pts',(13.7776094956075,0.546803061895555,4.35338757606046));
#22794=CARTESIAN_POINT('Ctrl Pts',(13.8012236117573,0.313543031018869,4.57058490613733));
#22795=CARTESIAN_POINT('Ctrl Pts',(13.8248377279072,0.00514023007941788,
4.65103759142385));
#22796=CARTESIAN_POINT('Ctrl Pts',(13.8484518440571,-0.304494462781446,
4.57546458583277));
#22797=CARTESIAN_POINT('Ctrl Pts',(13.8720659602069,-0.541154937947787,
4.36197748624323));
#22798=CARTESIAN_POINT('Ctrl Pts',(13.8956800763568,-0.648123865072376,
4.06173996222779));
#22799=CARTESIAN_POINT('Ctrl Pts',(13.9192941925067,-0.599765396122921,
3.74670602647169));
#22800=CARTESIAN_POINT('Ctrl Pts',(13.9429083086565,-0.407668974822819,
3.49237575473668));
#22801=CARTESIAN_POINT('Ctrl Pts',(13.9665224248064,-0.117871845784803,
3.35970116712309));
#22802=CARTESIAN_POINT('Ctrl Pts',(13.9901365409563,0.200174091641329,3.38047865214521));
#22803=CARTESIAN_POINT('Ctrl Pts',(14.0137506571061,0.470246914526057,3.54972874087838));
#22804=CARTESIAN_POINT('Ctrl Pts',(14.037364773256,0.627621790796785,3.82688947135059));
#22805=CARTESIAN_POINT('Ctrl Pts',(14.0609788894059,0.634582735815489,4.14553734509456));
#22806=CARTESIAN_POINT('Ctrl Pts',(14.0845930055557,0.489461510650943,4.42930618095194));
#22807=CARTESIAN_POINT('Ctrl Pts',(14.1082071217056,0.227037427151766,4.61018880199865));
#22808=CARTESIAN_POINT('Ctrl Pts',(14.1318212378555,-0.0897977562486571,
4.64483542891575));
#22809=CARTESIAN_POINT('Ctrl Pts',(14.1554353540053,-0.385112282251534,
4.52494275637564));
#22810=CARTESIAN_POINT('Ctrl Pts',(14.1790494701552,-0.588131968915973,
4.27924389796604));
#22811=CARTESIAN_POINT('Ctrl Pts',(14.2026635863051,-0.65020173504413,3.96662229549764));
#22812=CARTESIAN_POINT('Ctrl Pts',(14.2262777024549,-0.556446129094758,
3.66199989226673));
#22813=CARTESIAN_POINT('Ctrl Pts',(14.2498918186048,-0.329334334698108,
3.43838156778717));
#22814=CARTESIAN_POINT('Ctrl Pts',(14.2735059347547,-0.0232952743833569,
3.34935901020328));
#22815=CARTESIAN_POINT('Ctrl Pts',(14.2971200509045,0.28832666060365,3.41626709515619));
#22816=CARTESIAN_POINT('Ctrl Pts',(14.3207341670544,0.530849104237583,3.62307083431711));
#22817=CARTESIAN_POINT('Ctrl Pts',(14.3443482832043,0.646149864620809,3.92020827196535));
#22818=CARTESIAN_POINT('Ctrl Pts',(14.3679623993541,0.606596311879891,4.2364683526943));
#22819=CARTESIAN_POINT('Ctrl Pts',(14.391576515504,0.42166773027486,4.49605714656388));
#22820=CARTESIAN_POINT('Ctrl Pts',(14.4151906316539,0.135683541737747,4.63676239203782));
#22821=CARTESIAN_POINT('Ctrl Pts',(14.4388047478037,-0.182818152115814,
4.62486309754155));
#22822=CARTESIAN_POINT('Ctrl Pts',(14.4624188639536,-0.457506203155893,
4.46321101183598));
#22823=CARTESIAN_POINT('Ctrl Pts',(14.4860329801035,-0.622549707754089,
4.19054718257559));
#22824=CARTESIAN_POINT('Ctrl Pts',(14.5096470962533,-0.63839484111024,3.87221739454711));
#22825=CARTESIAN_POINT('Ctrl Pts',(14.5332612124032,-0.501244206711231,
3.58451159745434));
#22826=CARTESIAN_POINT('Ctrl Pts',(14.5568753285531,-0.243966908844842,
3.39638048838484));
#22827=CARTESIAN_POINT('Ctrl Pts',(14.5804894447029,0.0717787570654544,
3.35291099727801));
#22828=CARTESIAN_POINT('Ctrl Pts',(14.6041035608528,0.370322144162233,3.46452089026927));
#22829=CARTESIAN_POINT('Ctrl Pts',(14.6277176770027,0.580115251486915,3.70446207957941));
#22830=CARTESIAN_POINT('Ctrl Pts',(14.6513317931525,0.650879700384091,4.0152309888134));
#22831=CARTESIAN_POINT('Ctrl Pts',(14.6749459093024,0.565656298155129,4.32234968564526));
#22832=CARTESIAN_POINT('Ctrl Pts',(14.6985600254523,0.344869426209941,4.55221503612336));
#22833=CARTESIAN_POINT('Ctrl Pts',(14.7221741416021,0.041432195817608,4.64973820947522));
#22834=CARTESIAN_POINT('Ctrl Pts',(14.745788257752,-0.271934549361806,4.59154709694401));
#22835=CARTESIAN_POINT('Ctrl Pts',(14.7694023739019,-0.520130285395982,
4.39158760667368));
#22836=CARTESIAN_POINT('Ctrl Pts',(14.7930164900517,-0.64367318065081,4.09778141619902));
#22837=CARTESIAN_POINT('Ctrl Pts',(14.8166306062016,-0.612955311082805,
3.78054123783642));
#22838=CARTESIAN_POINT('Ctrl Pts',(14.8402447223515,-0.435338447621071,
3.51589585985611));
#22839=CARTESIAN_POINT('Ctrl Pts',(14.8638588385013,-0.153389665944836,
3.36726945127358));
#22840=CARTESIAN_POINT('Ctrl Pts',(14.8874729546512,0.165319955489652,3.37028123293502));
#22841=CARTESIAN_POINT('Ctrl Pts',(14.9110870708011,0.444409630539555,3.52420969451069));
#22842=CARTESIAN_POINT('Ctrl Pts',(14.9347011869509,0.616993161964042,3.79216419995926));
#22843=CARTESIAN_POINT('Ctrl Pts',(14.9583153031008,0.641710593195818,4.10992889087348));
#22844=CARTESIAN_POINT('Ctrl Pts',(14.9819294192507,0.512636325700993,4.40134645341462));
#22845=CARTESIAN_POINT('Ctrl Pts',(15.0055435354005,0.260708010403211,4.59658262768273));
#22846=CARTESIAN_POINT('Ctrl Pts',(15.0291576515504,-0.0537065278721878,
4.64883488988255));
#22847=CARTESIAN_POINT('Ctrl Pts',(15.0527717677003,-0.355236031271534,
4.54560815721762));
#22848=CARTESIAN_POINT('Ctrl Pts',(15.0763858838501,-0.571652475026301,
4.31158258982903));
#22849=CARTESIAN_POINT('Ctrl Pts',(15.09212862795,-0.624530364890795,4.10584538053252));
#22850=CARTESIAN_POINT('Ctrl Pts',(15.1,-0.624993681275899,4.00281040303152));
#22851=CARTESIAN_POINT('Ctrl Pts',(15.1,-0.624993681275899,4.00281040303152));
#22852=CARTESIAN_POINT('Ctrl Pts',(15.1,-0.617358358083874,4.02914127082806));
#22853=CARTESIAN_POINT('Ctrl Pts',(15.1,-0.607931963506944,4.05484759228836));
#22854=CARTESIAN_POINT('Ctrl Pts',(15.1,-0.596773861259576,4.07974656001827));
#22855=CARTESIAN_POINT('Ctrl Pts',(15.1,-0.585871522029423,4.10407480030985));
#22856=CARTESIAN_POINT('Ctrl Pts',(15.1,-0.573314772633929,4.12763281365198));
#22857=CARTESIAN_POINT('Ctrl Pts',(15.1,-0.559143639302279,4.1502040881484));
#22858=CARTESIAN_POINT('Ctrl Pts',(15.1,-0.549626121151564,4.16536325076984));
#22859=CARTESIAN_POINT('Ctrl Pts',(15.1,-0.539380106047495,4.18007635520315));
#22860=CARTESIAN_POINT('Ctrl Pts',(15.1,-0.528417753985571,4.19426420824267));
#22861=CARTESIAN_POINT('Ctrl Pts',(15.1,-0.523814643226911,4.2002217124899));
#22862=CARTESIAN_POINT('Ctrl Pts',(15.1,-0.519084627089791,4.20608691507751));
#22863=CARTESIAN_POINT('Ctrl Pts',(15.1,-0.514239086396905,4.21184190560023));
#22864=CARTESIAN_POINT('Ctrl Pts',(15.1,-0.50085552272952,4.2277374035328));
#22865=CARTESIAN_POINT('Ctrl Pts',(15.1,-0.486572803760524,4.24281789068328));
#22866=CARTESIAN_POINT('Ctrl Pts',(15.1,-0.4714177983537,4.25697008589974));
#22867=CARTESIAN_POINT('Ctrl Pts',(15.1,-0.457151696655403,4.27029219637033));
#22868=CARTESIAN_POINT('Ctrl Pts',(15.1,-0.442112042545397,4.28279146400573));
#22869=CARTESIAN_POINT('Ctrl Pts',(15.1,-0.426369607892924,4.29437520287289));
#22870=CARTESIAN_POINT('Ctrl Pts',(15.1,-0.419074661497203,4.29974303548351));
#22871=CARTESIAN_POINT('Ctrl Pts',(15.1,-0.411628924918527,4.30491398987477));
#22872=CARTESIAN_POINT('Ctrl Pts',(15.1,-0.404040271526401,4.30987739070861));
#22873=CARTESIAN_POINT('Ctrl Pts',(15.1,-0.398073367501634,4.31378007737535));
#22874=CARTESIAN_POINT('Ctrl Pts',(15.1,-0.392026704362881,4.31754881952869));
#22875=CARTESIAN_POINT('Ctrl Pts',(15.1,-0.385904261325812,4.32117966642505));
#22876=CARTESIAN_POINT('Ctrl Pts',(15.1,-0.366868686798561,4.33246850264191));
#22877=CARTESIAN_POINT('Ctrl Pts',(15.1,-0.347097727375919,4.34242824684389));
#22878=CARTESIAN_POINT('Ctrl Pts',(15.1,-0.326713262272485,4.3509180109496));
#22879=CARTESIAN_POINT('Ctrl Pts',(15.1,-0.308010762698638,4.35870726657947));
#22880=CARTESIAN_POINT('Ctrl Pts',(15.1,-0.288791261952878,4.36525839133365));
#22881=CARTESIAN_POINT('Ctrl Pts',(15.1,-0.269173508333929,4.37043259773196));
#22882=CARTESIAN_POINT('Ctrl Pts',(12.5,-0.186196943290592,3.58169363627332));
#22883=CARTESIAN_POINT('Ctrl Pts',(12.5,-0.170588484282379,3.56594316788148));
#22884=CARTESIAN_POINT('Ctrl Pts',(12.5,-0.153797667832464,3.55144458439849));
#22885=CARTESIAN_POINT('Ctrl Pts',(12.5,-0.136060690067392,3.53823162417247));
#22886=CARTESIAN_POINT('Ctrl Pts',(12.5,-0.117990710310259,3.5247705978929));
#22887=CARTESIAN_POINT('Ctrl Pts',(12.5,-0.0989385549429972,3.51264262455394));
#22888=CARTESIAN_POINT('Ctrl Pts',(12.5,-0.0790990435859813,3.5018744512649));
#22889=CARTESIAN_POINT('Ctrl Pts',(12.5,-0.0668145727052721,3.49520688224936));
#22890=CARTESIAN_POINT('Ctrl Pts',(12.5,-0.054227138249592,3.4890605701039));
#22891=CARTESIAN_POINT('Ctrl Pts',(12.5,-0.0413735013057162,3.4834433907237));
#22892=CARTESIAN_POINT('Ctrl Pts',(12.5,-0.0353493612034326,3.48081077586818));
#22893=CARTESIAN_POINT('Ctrl Pts',(12.5,-0.0292710672153644,3.47829647656688));
#22894=CARTESIAN_POINT('Ctrl Pts',(12.5,-0.0231507758853709,3.47590397706369));
#22895=CARTESIAN_POINT('Ctrl Pts',(12.5,-0.00211397253512804,3.467680423829));
#22896=CARTESIAN_POINT('Ctrl Pts',(12.5,0.0194422610390746,3.46088402724794));
#22897=CARTESIAN_POINT('Ctrl Pts',(12.5,0.0413436963816045,3.45552737346533));
#22898=CARTESIAN_POINT('Ctrl Pts',(12.5,0.0650920698750741,3.44971899548849));
#22899=CARTESIAN_POINT('Ctrl Pts',(12.5,0.089246474293393,3.44560199012534));
#22900=CARTESIAN_POINT('Ctrl Pts',(12.5,0.113633446029948,3.44311473184586));
#22901=CARTESIAN_POINT('Ctrl Pts',(12.5,0.123118497624279,3.44214733936417));
#22902=CARTESIAN_POINT('Ctrl Pts',(12.5,0.132642564327611,3.44142688205345));
#22903=CARTESIAN_POINT('Ctrl Pts',(12.5,0.142169452875131,3.44095138714122));
#22904=CARTESIAN_POINT('Ctrl Pts',(12.5,0.170359862108328,3.43954438042575));
#22905=CARTESIAN_POINT('Ctrl Pts',(12.5,0.19861482332424,3.44027367679077));
#22906=CARTESIAN_POINT('Ctrl Pts',(12.5,0.226679319731597,3.44302987267532));
#22907=CARTESIAN_POINT('Ctrl Pts',(12.5,0.254743816138955,3.44578606855986));
#22908=CARTESIAN_POINT('Ctrl Pts',(12.5,0.282619254593541,3.45056842907764));
#22909=CARTESIAN_POINT('Ctrl Pts',(12.5,0.310093463203745,3.45730861053194));
#22910=CARTESIAN_POINT('Ctrl Pts',(15.0699957084852,-1.05870731373636E-5,
4.45788944868556));
#22911=CARTESIAN_POINT('Ctrl Pts',(15.0634386537186,0.0628625045491076,
4.45782850550181));
#22912=CARTESIAN_POINT('Ctrl Pts',(15.0568815989521,0.125761012144406,4.44477074790967));
#22913=CARTESIAN_POINT('Ctrl Pts',(15.0503245441856,0.183365120595825,4.41959809737683));
#22914=CARTESIAN_POINT('Ctrl Pts',(15.0424531721356,0.252515583017112,4.38937975928409));
#22915=CARTESIAN_POINT('Ctrl Pts',(15.0345818000857,0.314036477612831,4.34170308552782));
#22916=CARTESIAN_POINT('Ctrl Pts',(15.0267104280357,0.360556892971808,4.28228266426341));
#22917=CARTESIAN_POINT('Ctrl Pts',(15.0188390559858,0.407077308330786,4.222862242999));
#22918=CARTESIAN_POINT('Ctrl Pts',(15.0109676839358,0.438597244453022,4.15169807422645));
#22919=CARTESIAN_POINT('Ctrl Pts',(15.0030963118859,0.45133921416074,4.07731692107955));
#22920=CARTESIAN_POINT('Ctrl Pts',(14.9952249398359,0.464081183868457,4.00293576793266));
#22921=CARTESIAN_POINT('Ctrl Pts',(14.9873535677859,0.458045187161657,3.92533763041141));
#22922=CARTESIAN_POINT('Ctrl Pts',(14.979482195736,0.433954739621328,3.85382131653551));
#22923=CARTESIAN_POINT('Ctrl Pts',(14.971610823686,0.409864292080999,3.78230500265962));
#22924=CARTESIAN_POINT('Ctrl Pts',(14.9637394516361,0.367719393707138,3.71687051242907));
#22925=CARTESIAN_POINT('Ctrl Pts',(14.9558680795861,0.312570095196614,3.66535860215541));
#22926=CARTESIAN_POINT('Ctrl Pts',(14.9479967075362,0.257420796686091,3.61384669188175));
#22927=CARTESIAN_POINT('Ctrl Pts',(14.9401253354862,0.189267098038905,3.57625736156498));
#22928=CARTESIAN_POINT('Ctrl Pts',(14.9322539634362,0.116275803938161,3.55709495786573));
#22929=CARTESIAN_POINT('Ctrl Pts',(14.9243825913863,0.0432845098374172,
3.53793255416647));
#22930=CARTESIAN_POINT('Ctrl Pts',(14.9165112193363,-0.0345443797168851,
3.53719707708475));
#22931=CARTESIAN_POINT('Ctrl Pts',(14.9086398472864,-0.107884770736704,
3.55497662303181));
#22932=CARTESIAN_POINT('Ctrl Pts',(14.9007684752364,-0.181225161756525,
3.57275616897888));
#22933=CARTESIAN_POINT('Ctrl Pts',(14.8928971031865,-0.250077054241862,
3.60905073795473));
#22934=CARTESIAN_POINT('Ctrl Pts',(14.8850257311365,-0.306190019513209,
3.65951122309406));
#22935=CARTESIAN_POINT('Ctrl Pts',(14.8771543590866,-0.362302984784554,
3.70997170823338));
#22936=CARTESIAN_POINT('Ctrl Pts',(14.8692829870366,-0.405677022841909,
3.77459810953617));
#22937=CARTESIAN_POINT('Ctrl Pts',(14.8614116149867,-0.431114693744839,
3.84564633596564));
#22938=CARTESIAN_POINT('Ctrl Pts',(14.8535402429367,-0.45655236464777,3.91669456239511));
#22939=CARTESIAN_POINT('Ctrl Pts',(14.8456688708867,-0.464053668396277,
3.99416461395126));
#22940=CARTESIAN_POINT('Ctrl Pts',(14.8377974988368,-0.452719732759917,
4.06877337558629));
#22941=CARTESIAN_POINT('Ctrl Pts',(14.8299261267868,-0.441385797123556,
4.14338213722132));
#22942=CARTESIAN_POINT('Ctrl Pts',(14.8220547547369,-0.411216622102327,
4.21512960893523));
#22943=CARTESIAN_POINT('Ctrl Pts',(14.8141833826869,-0.365827335221939,
4.27541839855419));
#22944=CARTESIAN_POINT('Ctrl Pts',(14.806312010637,-0.32043804834155,4.33570718817315));
#22945=CARTESIAN_POINT('Ctrl Pts',(14.798440638587,-0.259828649602004,4.38453729569717));
#22946=CARTESIAN_POINT('Ctrl Pts',(14.7905692665371,-0.191261870645823,
4.41605748429924));
#22947=CARTESIAN_POINT('Ctrl Pts',(14.7837114138531,-0.131523763221734,
4.44351912740692));
#22948=CARTESIAN_POINT('Ctrl Pts',(14.7768535611691,-0.065745536276614,
4.45784152413683));
#22949=CARTESIAN_POINT('Ctrl Pts',(14.7699957084852,8.6346448269735E-6,
4.45789857801605));
#22950=CARTESIAN_POINT('Ctrl Pts',(12.5,0.310062960217722,4.54266560670548));
#22951=CARTESIAN_POINT('Ctrl Pts',(12.50787137205,0.220600394030941,4.59378185169648));
#22952=CARTESIAN_POINT('Ctrl Pts',(12.5236141161499,0.0159878432799406,
4.65085692712531));
#22953=CARTESIAN_POINT('Ctrl Pts',(12.5472282322997,-0.294892507759568,
4.580447501361));
#22954=CARTESIAN_POINT('Ctrl Pts',(12.5708423484496,-0.535054221536356,
4.37092866956447));
#22955=CARTESIAN_POINT('Ctrl Pts',(12.5944564645995,-0.647009713430093,
4.07251155115386));
#22956=CARTESIAN_POINT('Ctrl Pts',(12.6180705807493,-0.603894380709874,
3.75671714932517));
#22957=CARTESIAN_POINT('Ctrl Pts',(12.6416846968992,-0.416056506175611,
3.49922677321964));
#22958=CARTESIAN_POINT('Ctrl Pts',(12.6652988130491,-0.128505496873939,
3.36175035317655));
#22959=CARTESIAN_POINT('Ctrl Pts',(12.6889129291989,0.189841674427298,3.37723482234205));
#22960=CARTESIAN_POINT('Ctrl Pts',(12.7125270453488,0.462692468193658,3.54196933898577));
#22961=CARTESIAN_POINT('Ctrl Pts',(12.7361411614987,0.624655556881011,3.81647407445394));
#22962=CARTESIAN_POINT('Ctrl Pts',(12.7597552776485,0.636915702199809,4.13496208375113));
#22963=CARTESIAN_POINT('Ctrl Pts',(12.7833693937984,0.496534514683115,4.42110548633398));
#22964=CARTESIAN_POINT('Ctrl Pts',(12.8069835099483,0.237155397994168,4.60632802944461));
#22965=CARTESIAN_POINT('Ctrl Pts',(12.8305976260981,-0.0790596718614395,
4.64623983861064));
#22966=CARTESIAN_POINT('Ctrl Pts',(12.854211742248,-0.376327535803878,4.5312757721487));
#22967=CARTESIAN_POINT('Ctrl Pts',(12.8778258583979,-0.583405888470749,
4.28898776831928));
#22968=CARTESIAN_POINT('Ctrl Pts',(12.9014399745477,-0.650666957548692,
3.97744183415536));
#22969=CARTESIAN_POINT('Ctrl Pts',(12.9250540906976,-0.561991161265395,
3.67130212143154));
#22970=CARTESIAN_POINT('Ctrl Pts',(12.9486682068475,-0.338630270727757,
3.44393714350224));
#22971=CARTESIAN_POINT('Ctrl Pts',(12.9722823229973,-0.0341142786054444,
3.34983650006563));
#22972=CARTESIAN_POINT('Ctrl Pts',(12.9958964391472,0.278577437919422,3.41155206540036));
#22973=CARTESIAN_POINT('Ctrl Pts',(13.0195105552971,0.524506132150044,3.61429327464512));
#22974=CARTESIAN_POINT('Ctrl Pts',(13.0431246714469,0.644733280558021,3.90947178565704));
#22975=CARTESIAN_POINT('Ctrl Pts',(13.0667387875968,0.61044561006836,4.22634601343335));
#22976=CARTESIAN_POINT('Ctrl Pts',(13.0903529037467,0.429860399609997,4.4889748434194));
#22977=CARTESIAN_POINT('Ctrl Pts',(13.1139670198965,0.146256151980267,4.63441744826062));
#22978=CARTESIAN_POINT('Ctrl Pts',(13.1375811360464,-0.172399400609521,
4.62781749523177));
#22979=CARTESIAN_POINT('Ctrl Pts',(13.1611952521963,-0.449738236712957,
4.47075670902068));
#22980=CARTESIAN_POINT('Ctrl Pts',(13.1848093683461,-0.619294173608025,
4.2008758003961));
#22981=CARTESIAN_POINT('Ctrl Pts',(13.208423484496,-0.64043195068177,3.88285360784221));
#22982=CARTESIAN_POINT('Ctrl Pts',(13.2320376006459,-0.508085752511173,
3.59290636366459));
#22983=CARTESIAN_POINT('Ctrl Pts',(13.2556517167957,-0.253973266794505,
3.40052194335125));
#22984=CARTESIAN_POINT('Ctrl Pts',(13.2792658329456,0.0610056803032868,
3.3518066124833));
#22985=CARTESIAN_POINT('Ctrl Pts',(13.3028799490955,0.361364191435218,3.45843533922715));
#22986=CARTESIAN_POINT('Ctrl Pts',(13.3264940652453,0.575119258511334,3.69485380694));
#22987=CARTESIAN_POINT('Ctrl Pts',(13.3501081813952,0.65104299168552,4.00440268404554));
#22988=CARTESIAN_POINT('Ctrl Pts',(13.3737222975451,0.570939739771795,4.31289642727099));
#22989=CARTESIAN_POINT('Ctrl Pts',(13.3973364136949,0.354006804717113,4.54640236352309));
#22990=CARTESIAN_POINT('Ctrl Pts',(13.4209505298448,0.0522336745508671,
4.6489591696652));
#22991=CARTESIAN_POINT('Ctrl Pts',(13.4445646459947,-0.26205761933777,4.59598839317277));
#22992=CARTESIAN_POINT('Ctrl Pts',(13.4681787621445,-0.513544980480383,
4.40018484937968));
#22993=CARTESIAN_POINT('Ctrl Pts',(13.4917928782944,-0.64195771209056,4.10847422061066));
#22994=CARTESIAN_POINT('Ctrl Pts',(13.5154069944443,-0.616520809113462,
3.79076698974655));
#22995=CARTESIAN_POINT('Ctrl Pts',(13.5390211105941,-0.443330402422436,
3.52320390633144));
#22996=CARTESIAN_POINT('Ctrl Pts',(13.562635226744,-0.163892778617988,3.36990832590288));
#22997=CARTESIAN_POINT('Ctrl Pts',(13.5862493428939,0.154822890495328,3.36761860145296));
#22998=CARTESIAN_POINT('Ctrl Pts',(13.6098634590437,0.43643417612693,3.51688348138565));
#22999=CARTESIAN_POINT('Ctrl Pts',(13.6334775751936,0.613450973283793,3.78193059814177));
#23000=CARTESIAN_POINT('Ctrl Pts',(13.6570916913435,0.643449974253473,4.09923956510808));
#23001=CARTESIAN_POINT('Ctrl Pts',(13.6807058074933,0.519241709620395,4.39276507945606));
#23002=CARTESIAN_POINT('Ctrl Pts',(13.7043199236432,0.270593554659618,4.59216170834183));
#23003=CARTESIAN_POINT('Ctrl Pts',(13.7279340397931,-0.0429042293685969,
4.64964266158552));
#23004=CARTESIAN_POINT('Ctrl Pts',(13.7515481559429,-0.346119716157775,
4.55143222859795));
#23005=CARTESIAN_POINT('Ctrl Pts',(13.7751622720928,-0.566385203513325,
4.32106722332061));
#23006=CARTESIAN_POINT('Ctrl Pts',(13.7987763882427,-0.650912534047929,
4.01375622291695));
#23007=CARTESIAN_POINT('Ctrl Pts',(13.8223905043925,-0.57944414457563,3.70314844792952));
#23008=CARTESIAN_POINT('Ctrl Pts',(13.8460046205424,-0.369107932149097,
3.46368321387984));
#23009=CARTESIAN_POINT('Ctrl Pts',(13.8696187366923,-0.0703124342978696,
3.35275003110641));
#23010=CARTESIAN_POINT('Ctrl Pts',(13.8932328528421,0.245333927901481,3.3969348091043));
#23011=CARTESIAN_POINT('Ctrl Pts',(13.916846968992,0.502184306426786,3.58564835824111));
#23012=CARTESIAN_POINT('Ctrl Pts',(13.9404610851419,0.638682720042094,3.87366416276737));
#23013=CARTESIAN_POINT('Ctrl Pts',(13.9640752012917,0.62211637371287,4.19195723015293));
#23014=CARTESIAN_POINT('Ctrl Pts',(13.9876893174416,0.456455507660852,4.46424641105313));
#23015=CARTESIAN_POINT('Ctrl Pts',(14.0113034335915,0.181401901656729,4.62527570776815));
#23016=CARTESIAN_POINT('Ctrl Pts',(14.0349175497413,-0.137125932879425,
4.63645332836083));
#23017=CARTESIAN_POINT('Ctrl Pts',(14.0585316658912,-0.422790583021024,
4.49510047824495));
#23018=CARTESIAN_POINT('Ctrl Pts',(14.0821457820411,-0.60713052675338,4.23509335195577));
#23019=CARTESIAN_POINT('Ctrl Pts',(14.1057598981909,-0.645967413308333,
3.91874446730605));
#23020=CARTESIAN_POINT('Ctrl Pts',(14.1293740143408,-0.529993712466286,
3.62186903671368));
#23021=CARTESIAN_POINT('Ctrl Pts',(14.1529881304907,-0.287003328966194,
3.41561532377041));
#23022=CARTESIAN_POINT('Ctrl Pts',(14.1766022466405,0.0247694002478971,
3.34941346658496));
#23023=CARTESIAN_POINT('Ctrl Pts',(14.2002163627904,0.330605970264406,3.43912920108534));
#23024=CARTESIAN_POINT('Ctrl Pts',(14.2238304789403,0.557210518047066,3.66326152695696));
#23025=CARTESIAN_POINT('Ctrl Pts',(14.2474445950901,0.650275686248857,3.96809557204375));
#23026=CARTESIAN_POINT('Ctrl Pts',(14.27105871124,0.587497759452106,4.28057573538778));
#23027=CARTESIAN_POINT('Ctrl Pts',(14.2946728273899,0.383921904832036,4.52581397056352));
#23028=CARTESIAN_POINT('Ctrl Pts',(14.3182869435397,0.088336493108731,4.64503722732482));
#23029=CARTESIAN_POINT('Ctrl Pts',(14.3419010596896,-0.22841937412829,4.6096728222354));
#23030=CARTESIAN_POINT('Ctrl Pts',(14.3655151758395,-0.490432948250941,
4.42819608115853));
#23031=CARTESIAN_POINT('Ctrl Pts',(14.3891292919893,-0.634910852255616,
4.14409916841427));
#23032=CARTESIAN_POINT('Ctrl Pts',(14.4127434081392,-0.627227950688033,
3.82546788683648));
#23033=CARTESIAN_POINT('Ctrl Pts',(14.4363575242891,-0.469225504392149,
3.54866444115539));
#23034=CARTESIAN_POINT('Ctrl Pts',(14.4599716404389,-0.198769899531221,
3.38002670405092));
#23035=CARTESIAN_POINT('Ctrl Pts',(14.4835857565888,0.11932229545683,3.35996988316441));
#23036=CARTESIAN_POINT('Ctrl Pts',(14.5071998727387,0.408818071695872,3.49330073524378));
#23037=CARTESIAN_POINT('Ctrl Pts',(14.5308139888885,0.600337751131954,3.74806559342675));
#23038=CARTESIAN_POINT('Ctrl Pts',(14.5544281050384,0.647982309355475,4.06320828594604));
#23039=CARTESIAN_POINT('Ctrl Pts',(14.5780422211883,0.540333396317157,4.36320267272319));
#23040=CARTESIAN_POINT('Ctrl Pts',(14.6016563373381,0.303189823409542,4.57615301060753));
#23041=CARTESIAN_POINT('Ctrl Pts',(14.625270453488,-0.00661530128860875,
4.65102426869959));
#23042=CARTESIAN_POINT('Ctrl Pts',(14.6488845696379,-0.314835022974042,
4.56987302880665));
#23043=CARTESIAN_POINT('Ctrl Pts',(14.6724986857877,-0.547602339746838,
4.35214775046202));
#23044=CARTESIAN_POINT('Ctrl Pts',(14.6961128019376,-0.649132943719538,
4.05002781234082));
#23045=CARTESIAN_POINT('Ctrl Pts',(14.7197269180875,-0.595094318970103,
3.73591836064326));
#23046=CARTESIAN_POINT('Ctrl Pts',(14.7433410342373,-0.398437197867616,
3.48509791236843));
#23047=CARTESIAN_POINT('Ctrl Pts',(14.7669551503872,-0.1062918289807,3.35767733339665));
#23048=CARTESIAN_POINT('Ctrl Pts',(14.7905692665371,0.211327117384507,3.38419385377023));
#23049=CARTESIAN_POINT('Ctrl Pts',(14.8141833826869,0.478300047385911,3.5582926020622));
#23050=CARTESIAN_POINT('Ctrl Pts',(14.8377974988368,0.630645044771057,3.83824960712979));
#23051=CARTESIAN_POINT('Ctrl Pts',(14.8614116149867,0.631851559871185,4.15697121131127));
#23052=CARTESIAN_POINT('Ctrl Pts',(14.8850257311365,0.481630465478622,4.4380735902585));
#23053=CARTESIAN_POINT('Ctrl Pts',(14.9086398472864,0.215983244330552,4.61418854455152));
#23054=CARTESIAN_POINT('Ctrl Pts',(14.9322539634363,-0.101425794369151,
4.64310902247508));
#23055=CARTESIAN_POINT('Ctrl Pts',(14.9558680795861,-0.394527586443172,
4.517903766532));
#23056=CARTESIAN_POINT('Ctrl Pts',(14.979482195736,-0.593077772790822,4.26857965265179));
#23057=CARTESIAN_POINT('Ctrl Pts',(15.0030963118859,-0.649493436571599,
3.95488773069898));
#23058=CARTESIAN_POINT('Ctrl Pts',(15.0267104280357,-0.550252000240565,
3.65200904506483));
#23059=CARTESIAN_POINT('Ctrl Pts',(15.0503245441856,-0.319142060764588,
3.43252503194012));
#23060=CARTESIAN_POINT('Ctrl Pts',(15.0739386603355,-0.0115409051696555,
3.34904846156061));
#23061=CARTESIAN_POINT('Ctrl Pts',(15.0975527764853,0.298810377697559,3.42155963907315));
#23062=CARTESIAN_POINT('Ctrl Pts',(15.1211668926352,0.537575400322941,3.63273573589665));
#23063=CARTESIAN_POINT('Ctrl Pts',(15.1369096367351,0.610790903144771,3.83214323401692));
#23064=CARTESIAN_POINT('Ctrl Pts',(15.1447810087851,0.621570310124627,3.93461384266089));
#23065=CARTESIAN_POINT('Ctrl Pts',(12.4850729970716,0.282426015030316,4.49429601229446));
#23066=CARTESIAN_POINT('Ctrl Pts',(12.4929443691216,0.200937545576316,4.54085609598193));
#23067=CARTESIAN_POINT('Ctrl Pts',(12.5086871132215,0.0145627935155885,
4.59284387968754));
#23068=CARTESIAN_POINT('Ctrl Pts',(12.5323012293714,-0.268607755567932,
4.52871028073968));
#23069=CARTESIAN_POINT('Ctrl Pts',(12.5559153455213,-0.487363055256749,
4.3378665608173));
#23070=CARTESIAN_POINT('Ctrl Pts',(12.5795294616711,-0.589339580973024,
4.06604835489435));
#23071=CARTESIAN_POINT('Ctrl Pts',(12.603143577821,-0.550067261575934,3.77840176074865));
#23072=CARTESIAN_POINT('Ctrl Pts',(12.6267576939709,-0.378972002925158,
3.54386236016666));
#23073=CARTESIAN_POINT('Ctrl Pts',(12.6503718101207,-0.117051373585908,
3.41863967169675));
#23074=CARTESIAN_POINT('Ctrl Pts',(12.6739859262706,0.172920453180012,3.43274395851062));
#23075=CARTESIAN_POINT('Ctrl Pts',(12.6976000424204,0.42145114619533,3.58279513857084));
#23076=CARTESIAN_POINT('Ctrl Pts',(12.7212141585703,0.568977924911017,3.83283235195095));
#23077=CARTESIAN_POINT('Ctrl Pts',(12.7448282747202,0.580145282610399,4.12293246335278));
#23078=CARTESIAN_POINT('Ctrl Pts',(12.76844239087,0.45227673827436,4.38357095065208));
#23079=CARTESIAN_POINT('Ctrl Pts',(12.7920565070199,0.216016946852954,4.55228399108678));
#23080=CARTESIAN_POINT('Ctrl Pts',(12.8156706231698,-0.0720128197761896,
4.58863832766248));
#23081=CARTESIAN_POINT('Ctrl Pts',(12.8392847393196,-0.34278420811256,4.48392139165784));
#23082=CARTESIAN_POINT('Ctrl Pts',(12.8628988554695,-0.531404976945056,
4.26322932523642));
#23083=CARTESIAN_POINT('Ctrl Pts',(12.8865129716194,-0.592670842732518,
3.97945251867098));
#23084=CARTESIAN_POINT('Ctrl Pts',(12.9101270877692,-0.51189901575794,3.70060005900794));
#23085=CARTESIAN_POINT('Ctrl Pts',(12.9337412039191,-0.308447025930223,
3.49350087944474));
#23086=CARTESIAN_POINT('Ctrl Pts',(12.957355320069,-0.0310735592390789,
3.40778774002645));
#23087=CARTESIAN_POINT('Ctrl Pts',(12.9809694362188,0.253746902286204,3.46400239130434));
#23088=CARTESIAN_POINT('Ctrl Pts',(13.0045835523687,0.477755152237737,3.64867260076509));
#23089=CARTESIAN_POINT('Ctrl Pts',(13.0281976685186,0.587266054150949,3.91754086716214));
#23090=CARTESIAN_POINT('Ctrl Pts',(13.0518117846685,0.556034558024266,4.20617103876933));
#23091=CARTESIAN_POINT('Ctrl Pts',(13.0754259008183,0.391545509324759,4.44539088570928));
#23092=CARTESIAN_POINT('Ctrl Pts',(13.0990400169682,0.133219853633759,4.57786970637232));
#23093=CARTESIAN_POINT('Ctrl Pts',(13.122654133118,-0.157032867368526,4.57185802915678));
#23094=CARTESIAN_POINT('Ctrl Pts',(13.1462682492679,-0.409651568547275,
4.42879659435664));
#23095=CARTESIAN_POINT('Ctrl Pts',(13.1698823654178,-0.564094419600429,
4.1829710707208));
#23096=CARTESIAN_POINT('Ctrl Pts',(13.1934964815676,-0.583348116144335,
3.89329525626321));
#23097=CARTESIAN_POINT('Ctrl Pts',(13.2171105977175,-0.462798375770677,
3.62919197644995));
#23098=CARTESIAN_POINT('Ctrl Pts',(13.2407247138674,-0.231335782947555,
3.45395542080054));
#23099=CARTESIAN_POINT('Ctrl Pts',(13.2643388300172,0.055568040665587,3.40958224975729));
#23100=CARTESIAN_POINT('Ctrl Pts',(13.2879529461671,0.329154596505292,3.50670680265737));
#23101=CARTESIAN_POINT('Ctrl Pts',(13.311567062317,0.523856961936024,3.72205250428141));
#23102=CARTESIAN_POINT('Ctrl Pts',(13.3351811784668,0.593013359693284,4.00401025814095));
#23103=CARTESIAN_POINT('Ctrl Pts',(13.3587952946167,0.520049977633468,4.28500692572024));
#23104=CARTESIAN_POINT('Ctrl Pts',(13.3824094107666,0.322452998189994,4.49769969952106));
#23105=CARTESIAN_POINT('Ctrl Pts',(13.4060235269164,0.0475779130258999,
4.59111527567571));
#23106=CARTESIAN_POINT('Ctrl Pts',(13.4296376430663,-0.238699550200797,
4.5428659610613));
#23107=CARTESIAN_POINT('Ctrl Pts',(13.4532517592162,-0.467771004553565,
4.36451503980497));
#23108=CARTESIAN_POINT('Ctrl Pts',(13.476865875366,-0.584737881352888,4.09880555174689));
#23109=CARTESIAN_POINT('Ctrl Pts',(13.5004799915159,-0.561568254327815,
3.80941662539381));
#23110=CARTESIAN_POINT('Ctrl Pts',(13.5240941076658,-0.403814885886516,
3.56570233148043));
#23111=CARTESIAN_POINT('Ctrl Pts',(13.5477082238157,-0.149284468950505,
3.42607049712074));
#23112=CARTESIAN_POINT('Ctrl Pts',(13.5713223399655,0.141023010189178,3.42398486344345));
#23113=CARTESIAN_POINT('Ctrl Pts',(13.5949364561154,0.39753334322815,3.55994526707815));
#23114=CARTESIAN_POINT('Ctrl Pts',(13.6185505722652,0.55877204319843,3.8013678508274));
#23115=CARTESIAN_POINT('Ctrl Pts',(13.6421646884151,0.586097133215014,4.09039401187145));
#23116=CARTESIAN_POINT('Ctrl Pts',(13.665778804565,0.47295996523623,4.35775661870721));
#23117=CARTESIAN_POINT('Ctrl Pts',(13.6893929207148,0.24647464915429,4.53938036140496));
#23118=CARTESIAN_POINT('Ctrl Pts',(13.7130070368647,-0.0390800323908759,
4.59173784568287));
#23119=CARTESIAN_POINT('Ctrl Pts',(13.7366211530146,-0.315268912124245,
4.50228123595558));
#23120=CARTESIAN_POINT('Ctrl Pts',(13.7602352691644,-0.515901402373503,
4.29244943148197));
#23121=CARTESIAN_POINT('Ctrl Pts',(13.7838493853143,-0.59289453017979,4.01253008491428));
#23122=CARTESIAN_POINT('Ctrl Pts',(13.8074635014642,-0.527796356489121,
3.72960781627073));
#23123=CARTESIAN_POINT('Ctrl Pts',(13.831077617614,-0.336208111796874,3.51148691674935));
#23124=CARTESIAN_POINT('Ctrl Pts',(13.8546917337639,-0.0640452526541193,
3.4104415783338));
#23125=CARTESIAN_POINT('Ctrl Pts',(13.8783058499138,0.223466497127862,3.45068801978614));
#23126=CARTESIAN_POINT('Ctrl Pts',(13.9019199660636,0.457422945247278,3.62258090124322));
#23127=CARTESIAN_POINT('Ctrl Pts',(13.9255340822135,0.581754800262342,3.88492489705937));
#23128=CARTESIAN_POINT('Ctrl Pts',(13.9491481983634,0.566665067602596,4.17484744237197));
#23129=CARTESIAN_POINT('Ctrl Pts',(13.9727623145132,0.415770106744681,4.42286658094793));
#23130=CARTESIAN_POINT('Ctrl Pts',(13.9963764306631,0.165232945489059,4.56954279968241));
#23131=CARTESIAN_POINT('Ctrl Pts',(14.019990546813,-0.124903441395439,4.57972412169294));
#23132=CARTESIAN_POINT('Ctrl Pts',(14.0436046629628,-0.385105849054417,
4.45097052228405));
#23133=CARTESIAN_POINT('Ctrl Pts',(14.0672187791127,-0.553014959135429,
4.21413869785145));
#23134=CARTESIAN_POINT('Ctrl Pts',(14.0908328952626,-0.58839018453545,3.92598704378684));
#23135=CARTESIAN_POINT('Ctrl Pts',(14.1144470114124,-0.482753606228458,
3.65557310990793));
#23136=CARTESIAN_POINT('Ctrl Pts',(14.1380611275623,-0.261421765577673,
3.46770347791168));
#23137=CARTESIAN_POINT('Ctrl Pts',(14.1616752437122,0.0225616210391343,
3.40740241293002));
#23138=CARTESIAN_POINT('Ctrl Pts',(14.185289359862,0.301137958114838,3.48912148496193));
#23139=CARTESIAN_POINT('Ctrl Pts',(14.2089034760119,0.507544487205137,3.69327614952086));
#23140=CARTESIAN_POINT('Ctrl Pts',(14.2325175921618,0.592314446747875,3.97093932005559));
#23141=CARTESIAN_POINT('Ctrl Pts',(14.2561317083116,0.535132125826274,4.25556708484021));
#23142=CARTESIAN_POINT('Ctrl Pts',(14.2797458244615,0.349701665714674,4.47894641865396));
#23143=CARTESIAN_POINT('Ctrl Pts',(14.3033599406114,0.0804627670229728,
4.58754290912926));
#23144=CARTESIAN_POINT('Ctrl Pts',(14.3269740567612,-0.208059593914322,
4.55533065134682));
#23145=CARTESIAN_POINT('Ctrl Pts',(14.3505881729111,-0.44671902479684,4.39002953712461));
#23146=CARTESIAN_POINT('Ctrl Pts',(14.374202289061,-0.578319131624566,4.13125512920294));
#23147=CARTESIAN_POINT('Ctrl Pts',(14.3978164052108,-0.571321032683373,
3.84102451585645));
#23148=CARTESIAN_POINT('Ctrl Pts',(14.4214305213607,-0.427401871100662,
3.58889348396707));
#23149=CARTESIAN_POINT('Ctrl Pts',(14.4450446375106,-0.181052875819672,
3.43528699049651));
#23150=CARTESIAN_POINT('Ctrl Pts',(14.4686587536604,0.108686701521778,3.41701790091169));
#23151=CARTESIAN_POINT('Ctrl Pts',(14.4922728698103,0.372378754238714,3.53846452970905));
#23152=CARTESIAN_POINT('Ctrl Pts',(14.5158869859602,0.546827646247725,3.77052134686598));
#23153=CARTESIAN_POINT('Ctrl Pts',(14.53950110211,0.59022548618159,4.05757432072539));
#23154=CARTESIAN_POINT('Ctrl Pts',(14.5631152182599,0.492171679592087,4.3308292078278));
#23155=CARTESIAN_POINT('Ctrl Pts',(14.5867293344098,0.276165503816305,4.52479857226205));
#23156=CARTESIAN_POINT('Ctrl Pts',(14.6103434505596,-0.00602565743375084,
4.59299630554951));
#23157=CARTESIAN_POINT('Ctrl Pts',(14.6339575667095,-0.286772727926288,
4.51907834617235));
#23158=CARTESIAN_POINT('Ctrl Pts',(14.6575716828594,-0.49879271786407,4.32075964763751));
#23159=CARTESIAN_POINT('Ctrl Pts',(14.6811857990092,-0.591273560669336,
4.04556866666751));
#23160=CARTESIAN_POINT('Ctrl Pts',(14.7047999151591,-0.542051578672567,
3.75945683743125));
#23161=CARTESIAN_POINT('Ctrl Pts',(14.728414031309,-0.362923162297683,3.53099285177933));
#23162=CARTESIAN_POINT('Ctrl Pts',(14.7520281474588,-0.0968176839575538,
3.41492969374656));
#23163=CARTESIAN_POINT('Ctrl Pts',(14.7756422636087,0.192490826988301,3.43908270827084));
#23164=CARTESIAN_POINT('Ctrl Pts',(14.7992563797586,0.435667569828913,3.59766345479839));
#23165=CARTESIAN_POINT('Ctrl Pts',(14.8228704959084,0.574433549780463,3.85266695881428));
#23166=CARTESIAN_POINT('Ctrl Pts',(14.8464846120583,0.575532524168,4.14297984400973));
#23167=CARTESIAN_POINT('Ctrl Pts',(14.8700987282082,0.438701136655627,4.39902663091346));
#23168=CARTESIAN_POINT('Ctrl Pts',(14.893712844358,0.196731937819222,4.55944387228049));
#23169=CARTESIAN_POINT('Ctrl Pts',(14.9173269605079,-0.0923853752310475,
4.58578657160514));
#23170=CARTESIAN_POINT('Ctrl Pts',(14.9409410766578,-0.359362027571537,
4.47174127747511));
#23171=CARTESIAN_POINT('Ctrl Pts',(14.9645551928076,-0.540214773976066,
4.24464025294543));
#23172=CARTESIAN_POINT('Ctrl Pts',(14.9881693089575,-0.59160192159185,3.95890873763601));
#23173=CARTESIAN_POINT('Ctrl Pts',(15.0117834251074,-0.501206205285789,
3.68302663884805));
#23174=CARTESIAN_POINT('Ctrl Pts',(15.0353975412572,-0.290695865081771,
3.48310596742652));
#23175=CARTESIAN_POINT('Ctrl Pts',(15.0590116574071,-0.0105122258222001,
3.40706994202017));
#23176=CARTESIAN_POINT('Ctrl Pts',(15.082625773557,0.272176412698783,3.47311795657709));
#23177=CARTESIAN_POINT('Ctrl Pts',(15.1062398897068,0.489659512974156,3.66547122397039));
#23178=CARTESIAN_POINT('Ctrl Pts',(15.1219826338067,0.5563490739778,3.84710486709154));
#23179=CARTESIAN_POINT('Ctrl Pts',(15.1298540058567,0.566167676482186,3.94044192881839));
#23180=CARTESIAN_POINT('Ctrl Pts',(12.4701459941433,0.254789069842909,4.44592641788345));
#23181=CARTESIAN_POINT('Ctrl Pts',(12.4780173661933,0.181274697121691,4.48793034026739));
#23182=CARTESIAN_POINT('Ctrl Pts',(12.4937601102932,0.0131377437512366,
4.53483083224977));
#23183=CARTESIAN_POINT('Ctrl Pts',(12.517374226443,-0.242323003376296,4.47697306011837));
#23184=CARTESIAN_POINT('Ctrl Pts',(12.5409883425929,-0.439671888977142,
4.30480445207012));
#23185=CARTESIAN_POINT('Ctrl Pts',(12.5646024587428,-0.531669448515955,
4.05958515863483));
#23186=CARTESIAN_POINT('Ctrl Pts',(12.5882165748926,-0.496240142441994,
3.80008637217214));
#23187=CARTESIAN_POINT('Ctrl Pts',(12.6118306910425,-0.341887499674706,
3.58849794711368));
#23188=CARTESIAN_POINT('Ctrl Pts',(12.6354448071924,-0.105597250297878,
3.47552899021694));
#23189=CARTESIAN_POINT('Ctrl Pts',(12.6590589233422,0.155999231932725,3.4882530946792));
#23190=CARTESIAN_POINT('Ctrl Pts',(12.6826730394921,0.380209824197002,3.62362093815591));
#23191=CARTESIAN_POINT('Ctrl Pts',(12.706287155642,0.513300292941022,3.84919062944795));
#23192=CARTESIAN_POINT('Ctrl Pts',(12.7299012717918,0.52337486302099,4.11090284295443));
#23193=CARTESIAN_POINT('Ctrl Pts',(12.7535153879417,0.408018961865605,4.34603641497018));
#23194=CARTESIAN_POINT('Ctrl Pts',(12.7771295040916,0.194878495711741,4.49823995272895));
#23195=CARTESIAN_POINT('Ctrl Pts',(12.8007436202414,-0.0649659676909401,
4.53103681671432));
#23196=CARTESIAN_POINT('Ctrl Pts',(12.8243577363913,-0.30924088042124,4.43656701116699));
#23197=CARTESIAN_POINT('Ctrl Pts',(12.8479718525412,-0.479404065419363,
4.23747088215356));
#23198=CARTESIAN_POINT('Ctrl Pts',(12.871585968691,-0.534674727916345,3.9814632031866));
#23199=CARTESIAN_POINT('Ctrl Pts',(12.8952000848409,-0.461806870250484,
3.72989799658434));
#23200=CARTESIAN_POINT('Ctrl Pts',(12.9188142009908,-0.278263781132688,
3.54306461538724));
#23201=CARTESIAN_POINT('Ctrl Pts',(12.9424283171406,-0.0280328398727138,
3.46573897998727));
#23202=CARTESIAN_POINT('Ctrl Pts',(12.9660424332905,0.228916366652986,3.51645271720832));
#23203=CARTESIAN_POINT('Ctrl Pts',(12.9896565494404,0.431004172325429,3.68305192688505));
#23204=CARTESIAN_POINT('Ctrl Pts',(13.0132706655902,0.529798827743877,3.92560994866724));
#23205=CARTESIAN_POINT('Ctrl Pts',(13.0368847817401,0.501623505980173,4.1859960641053));
#23206=CARTESIAN_POINT('Ctrl Pts',(13.06049889789,0.353230619039521,4.40180692799916));
#23207=CARTESIAN_POINT('Ctrl Pts',(13.0841130140398,0.120183555287252,4.52132196448402));
#23208=CARTESIAN_POINT('Ctrl Pts',(13.1077271301897,-0.14166633412753,4.51589856308179));
#23209=CARTESIAN_POINT('Ctrl Pts',(13.1313412463396,-0.369564900381594,
4.38683647969259));
#23210=CARTESIAN_POINT('Ctrl Pts',(13.1549553624894,-0.508894665592834,
4.16506634104549));
#23211=CARTESIAN_POINT('Ctrl Pts',(13.1785694786393,-0.5262642816069,3.9037369046842));
#23212=CARTESIAN_POINT('Ctrl Pts',(13.2021835947892,-0.417510999030181,
3.66547758923531));
#23213=CARTESIAN_POINT('Ctrl Pts',(13.225797710939,-0.208698299100604,3.50738889824983));
#23214=CARTESIAN_POINT('Ctrl Pts',(13.2494118270889,0.0501304010278875,
3.46735788703128));
#23215=CARTESIAN_POINT('Ctrl Pts',(13.2730259432388,0.296945001575366,3.55497826608759));
#23216=CARTESIAN_POINT('Ctrl Pts',(13.2966400593886,0.472594665360713,3.74925120162283));
#23217=CARTESIAN_POINT('Ctrl Pts',(13.3202541755385,0.534983727701048,4.00361783223636));
#23218=CARTESIAN_POINT('Ctrl Pts',(13.3438682916884,0.469160215495142,4.25711742416948));
#23219=CARTESIAN_POINT('Ctrl Pts',(13.3674824078382,0.290899191662876,4.44899703551904));
#23220=CARTESIAN_POINT('Ctrl Pts',(13.3910965239881,0.0429221515009326,
4.53327138168622));
#23221=CARTESIAN_POINT('Ctrl Pts',(13.414710640138,-0.215341481063824,4.48974352894983));
#23222=CARTESIAN_POINT('Ctrl Pts',(13.4383247562878,-0.421997028626747,
4.32884523023027));
#23223=CARTESIAN_POINT('Ctrl Pts',(13.4619388724377,-0.527518050615216,
4.08913688288313));
#23224=CARTESIAN_POINT('Ctrl Pts',(13.4855529885876,-0.506615699542168,
3.82806626104107));
#23225=CARTESIAN_POINT('Ctrl Pts',(13.5091671047374,-0.364299369350597,
3.60820075662942));
#23226=CARTESIAN_POINT('Ctrl Pts',(13.5327812208873,-0.134676159283021,
3.48223266833859));
#23227=CARTESIAN_POINT('Ctrl Pts',(13.5563953370372,0.127223129883027,3.48035112543394));
#23228=CARTESIAN_POINT('Ctrl Pts',(13.580009453187,0.35863251032937,3.60300705277064));
#23229=CARTESIAN_POINT('Ctrl Pts',(13.6036235693369,0.504093113113068,3.82080510351303));
#23230=CARTESIAN_POINT('Ctrl Pts',(13.6272376854868,0.528744292176554,4.08154845863482));
#23231=CARTESIAN_POINT('Ctrl Pts',(13.6508518016366,0.426678220852065,4.32274815795836));
#23232=CARTESIAN_POINT('Ctrl Pts',(13.6744659177865,0.222355743648963,4.48659901446809));
#23233=CARTESIAN_POINT('Ctrl Pts',(13.6980800339364,-0.0352558354131549,
4.53383302978021));
#23234=CARTESIAN_POINT('Ctrl Pts',(13.7216941500862,-0.284418108090716,
4.45313024331322));
#23235=CARTESIAN_POINT('Ctrl Pts',(13.7453082662361,-0.465417601233682,
4.26383163964332));
#23236=CARTESIAN_POINT('Ctrl Pts',(13.768922382386,-0.534876526311652,4.01130394691162));
#23237=CARTESIAN_POINT('Ctrl Pts',(13.7925364985358,-0.476148568402614,
3.75606718461195));
#23238=CARTESIAN_POINT('Ctrl Pts',(13.8161506146857,-0.303308291444651,
3.55929061961886));
#23239=CARTESIAN_POINT('Ctrl Pts',(13.8397647308356,-0.0577780710103693,
3.46813312556118));
#23240=CARTESIAN_POINT('Ctrl Pts',(13.8633788469854,0.201599066354243,3.50444123046797));
#23241=CARTESIAN_POINT('Ctrl Pts',(13.8869929631353,0.412661584067771,3.65951344424533));
#23242=CARTESIAN_POINT('Ctrl Pts',(13.9106070792852,0.52482688048259,3.89618563135138));
#23243=CARTESIAN_POINT('Ctrl Pts',(13.934221195435,0.511213761492322,4.157737654591));
#23244=CARTESIAN_POINT('Ctrl Pts',(13.9578353115849,0.375084705828511,4.38148675084272));
#23245=CARTESIAN_POINT('Ctrl Pts',(13.9814494277348,0.149063989321389,4.51380989159668));
#23246=CARTESIAN_POINT('Ctrl Pts',(14.0050635438846,-0.112680949911453,
4.52299491502504));
#23247=CARTESIAN_POINT('Ctrl Pts',(14.0286776600345,-0.347421115087809,
4.40684056632315));
#23248=CARTESIAN_POINT('Ctrl Pts',(14.0522917761844,-0.498899391517477,
4.19318404374712));
#23249=CARTESIAN_POINT('Ctrl Pts',(14.0759058923342,-0.530812955762567,
3.93322962026762));
#23250=CARTESIAN_POINT('Ctrl Pts',(14.0995200084841,-0.435513499990629,
3.68927718310219));
#23251=CARTESIAN_POINT('Ctrl Pts',(14.123134124634,-0.235840202189154,3.51979163205294));
#23252=CARTESIAN_POINT('Ctrl Pts',(14.1467482407838,0.020353841830372,3.46539135927508));
#23253=CARTESIAN_POINT('Ctrl Pts',(14.1703623569337,0.271669945965271,3.53911376883853));
#23254=CARTESIAN_POINT('Ctrl Pts',(14.1939764730836,0.457878456363209,3.72329077208477));
#23255=CARTESIAN_POINT('Ctrl Pts',(14.2175905892334,0.534353207246894,3.97378306806742));
#23256=CARTESIAN_POINT('Ctrl Pts',(14.2412047053833,0.482766492200443,4.23055843429265));
#23257=CARTESIAN_POINT('Ctrl Pts',(14.2648188215332,0.315481426597312,4.4320788667444));
#23258=CARTESIAN_POINT('Ctrl Pts',(14.288432937683,0.0725890409372144,4.53004859093371));
#23259=CARTESIAN_POINT('Ctrl Pts',(14.3120470538329,-0.187699813700353,
4.50098848045824));
#23260=CARTESIAN_POINT('Ctrl Pts',(14.3356611699828,-0.40300510134274,4.35186299309067));
#23261=CARTESIAN_POINT('Ctrl Pts',(14.3592752861326,-0.521727410993515,
4.11841108999162));
#23262=CARTESIAN_POINT('Ctrl Pts',(14.3828894022825,-0.515414114678713,
3.85658114487643));
#23263=CARTESIAN_POINT('Ctrl Pts',(14.4065035184324,-0.385578237809175,
3.62912252677875));
#23264=CARTESIAN_POINT('Ctrl Pts',(14.4301176345822,-0.163335852108122,
3.49054727694211));
#23265=CARTESIAN_POINT('Ctrl Pts',(14.4537317507321,0.0980511075867261,
3.47406591865897));
#23266=CARTESIAN_POINT('Ctrl Pts',(14.477345866882,0.335939436781555,3.58362832417432));
#23267=CARTESIAN_POINT('Ctrl Pts',(14.5009599830318,0.493317541363497,3.79297710030521));
#23268=CARTESIAN_POINT('Ctrl Pts',(14.5245740991817,0.532468663007706,4.05194035550473));
#23269=CARTESIAN_POINT('Ctrl Pts',(14.5481882153316,0.444009962867018,4.2984557429324));
#23270=CARTESIAN_POINT('Ctrl Pts',(14.5718023314814,0.249141184223067,4.47344413391656));
#23271=CARTESIAN_POINT('Ctrl Pts',(14.5954164476313,-0.00543601357889273,
4.53496834239941));
#23272=CARTESIAN_POINT('Ctrl Pts',(14.6190305637812,-0.258710432878536,
4.46828366353805));
#23273=CARTESIAN_POINT('Ctrl Pts',(14.642644679931,-0.449983095981302,4.28937154481299));
#23274=CARTESIAN_POINT('Ctrl Pts',(14.6662587960809,-0.533414177619135,
4.0411095209942));
#23275=CARTESIAN_POINT('Ctrl Pts',(14.6898729122308,-0.489008838375032,
3.78299531421925));
#23276=CARTESIAN_POINT('Ctrl Pts',(14.7134870283806,-0.327409126727749,
3.57688779119022));
#23277=CARTESIAN_POINT('Ctrl Pts',(14.7371011445305,-0.0873435389344073,
3.47218205409647));
#23278=CARTESIAN_POINT('Ctrl Pts',(14.7607152606804,0.173654536592096,3.49397156277145));
#23279=CARTESIAN_POINT('Ctrl Pts',(14.7843293768302,0.393035092271916,3.63703430753458));
#23280=CARTESIAN_POINT('Ctrl Pts',(14.8079434929801,0.518222054789869,3.86708431049878));
#23281=CARTESIAN_POINT('Ctrl Pts',(14.8315576091299,0.519213488464815,4.12898847670818));
#23282=CARTESIAN_POINT('Ctrl Pts',(14.8551717252798,0.395771807832633,4.35997967156842));
#23283=CARTESIAN_POINT('Ctrl Pts',(14.8787858414297,0.177480631307892,4.50469920000947));
#23284=CARTESIAN_POINT('Ctrl Pts',(14.9023999575796,-0.0833449560929437,
4.52846412073519));
#23285=CARTESIAN_POINT('Ctrl Pts',(14.9260140737294,-0.324196468699902,
4.42557878841823));
#23286=CARTESIAN_POINT('Ctrl Pts',(14.9496281898793,-0.487351775161311,
4.22070085323907));
#23287=CARTESIAN_POINT('Ctrl Pts',(14.9732423060292,-0.533710406612102,
3.96292974457304));
#23288=CARTESIAN_POINT('Ctrl Pts',(14.996856422179,-0.452160410331013,3.71404423263127));
#23289=CARTESIAN_POINT('Ctrl Pts',(15.0204705383289,-0.262249669398955,
3.53368690291293));
#23290=CARTESIAN_POINT('Ctrl Pts',(15.0440846544788,-0.0094835464747447,
3.46509142247974));
#23291=CARTESIAN_POINT('Ctrl Pts',(15.0676987706286,0.245542447700007,3.52467627408104));
#23292=CARTESIAN_POINT('Ctrl Pts',(15.0913128867785,0.441743625625371,3.69820671204414));
#23293=CARTESIAN_POINT('Ctrl Pts',(15.1070556308784,0.501907244810829,3.86206650016617));
#23294=CARTESIAN_POINT('Ctrl Pts',(15.1149270029284,0.510765042839744,3.94627001497588));
#23295=CARTESIAN_POINT('Ctrl Pts',(12.4552189912149,0.227152124655503,4.39755682347243));
#23296=CARTESIAN_POINT('Ctrl Pts',(12.4630903632649,0.161611848667067,4.43500458455284));
#23297=CARTESIAN_POINT('Ctrl Pts',(12.4788331073648,0.0117126939868845,
4.476817784812));
#23298=CARTESIAN_POINT('Ctrl Pts',(12.5024472235147,-0.216038251184659,
4.42523583949706));
#23299=CARTESIAN_POINT('Ctrl Pts',(12.5260613396645,-0.391980722697534,
4.27174234332294));
#23300=CARTESIAN_POINT('Ctrl Pts',(12.5496754558144,-0.473999316058885,
4.05312196237532));
#23301=CARTESIAN_POINT('Ctrl Pts',(12.5732895719643,-0.442413023308054,
3.82177098359562));
#23302=CARTESIAN_POINT('Ctrl Pts',(12.5969036881141,-0.304802996424253,
3.6331335340607));
#23303=CARTESIAN_POINT('Ctrl Pts',(12.620517804264,-0.0941431270098475,
3.53241830873714));
#23304=CARTESIAN_POINT('Ctrl Pts',(12.6441319204139,0.139078010685439,3.54376223084778));
#23305=CARTESIAN_POINT('Ctrl Pts',(12.6677460365637,0.338968502198674,3.66444673774097));
#23306=CARTESIAN_POINT('Ctrl Pts',(12.6913601527136,0.457622660971028,3.86554890694496));
#23307=CARTESIAN_POINT('Ctrl Pts',(12.7149742688635,0.46660444343158,4.09887322255608));
#23308=CARTESIAN_POINT('Ctrl Pts',(12.7385883850133,0.36376118545685,4.30850187928827));
#23309=CARTESIAN_POINT('Ctrl Pts',(12.7622025011632,0.173740044570527,4.44419591437112));
#23310=CARTESIAN_POINT('Ctrl Pts',(12.7858166173131,-0.0579191156056905,
4.47343530576616));
#23311=CARTESIAN_POINT('Ctrl Pts',(12.809430733463,-0.275697552729921,4.38921263067613));
#23312=CARTESIAN_POINT('Ctrl Pts',(12.8330448496128,-0.42740315389367,4.2117124390707));
#23313=CARTESIAN_POINT('Ctrl Pts',(12.8566589657627,-0.476678613100171,
3.98347388770222));
#23314=CARTESIAN_POINT('Ctrl Pts',(12.8802730819125,-0.411714724743029,
3.75919593416074));
#23315=CARTESIAN_POINT('Ctrl Pts',(12.9038871980624,-0.248080536335154,
3.59262835132974));
#23316=CARTESIAN_POINT('Ctrl Pts',(12.9275013142123,-0.0249921205063485,
3.52369021994808));
#23317=CARTESIAN_POINT('Ctrl Pts',(12.9511154303621,0.204085831019768,3.5689030431123));
#23318=CARTESIAN_POINT('Ctrl Pts',(12.974729546512,0.384253192413122,3.71743125300502));
#23319=CARTESIAN_POINT('Ctrl Pts',(12.9983436626619,0.472331601336806,3.93367903017235));
#23320=CARTESIAN_POINT('Ctrl Pts',(13.0219577788117,0.44721245393608,4.16582108944128));
#23321=CARTESIAN_POINT('Ctrl Pts',(13.0455718949616,0.314915728754283,4.35822297028905));
#23322=CARTESIAN_POINT('Ctrl Pts',(13.0691860111115,0.107147256940744,4.46477422259573));
#23323=CARTESIAN_POINT('Ctrl Pts',(13.0928001272613,-0.126299800886535,
4.4599390970068));
#23324=CARTESIAN_POINT('Ctrl Pts',(13.1164142434112,-0.329478232215912,
4.34487636502855));
#23325=CARTESIAN_POINT('Ctrl Pts',(13.1400283595611,-0.453694911585238,
4.14716161137019));
#23326=CARTESIAN_POINT('Ctrl Pts',(13.1636424757109,-0.469180447069464,
3.9141785531052));
#23327=CARTESIAN_POINT('Ctrl Pts',(13.1872565918608,-0.372223622289685,
3.70176320202068));
#23328=CARTESIAN_POINT('Ctrl Pts',(13.2108707080107,-0.186060815253654,
3.56082237569912));
#23329=CARTESIAN_POINT('Ctrl Pts',(13.2344848241605,0.0446927613901878,
3.52513352430527));
#23330=CARTESIAN_POINT('Ctrl Pts',(13.2580989403104,0.26473540664544,3.60324972951781));
#23331=CARTESIAN_POINT('Ctrl Pts',(13.2817130564603,0.421332368785403,3.77644989896424));
#23332=CARTESIAN_POINT('Ctrl Pts',(13.3053271726101,0.476954095708811,4.00322540633176));
#23333=CARTESIAN_POINT('Ctrl Pts',(13.32894128876,0.418270453356816,4.22922792261873));
#23334=CARTESIAN_POINT('Ctrl Pts',(13.3525554049099,0.259345385135757,4.40029437151701));
#23335=CARTESIAN_POINT('Ctrl Pts',(13.3761695210597,0.0382663899759653,
4.47542748769673));
#23336=CARTESIAN_POINT('Ctrl Pts',(13.3997836372096,-0.19198341192685,4.43662109683837));
#23337=CARTESIAN_POINT('Ctrl Pts',(13.4233977533595,-0.376223052699929,
4.29317542065556));
#23338=CARTESIAN_POINT('Ctrl Pts',(13.4470118695093,-0.470298219877544,
4.07946821401937));
#23339=CARTESIAN_POINT('Ctrl Pts',(13.4706259856592,-0.451663144756522,
3.84671589668833));
#23340=CARTESIAN_POINT('Ctrl Pts',(13.4942401018091,-0.324783852814677,
3.65069918177841));
#23341=CARTESIAN_POINT('Ctrl Pts',(13.5178542179589,-0.120067849615538,
3.53839483955645));
#23342=CARTESIAN_POINT('Ctrl Pts',(13.5414683341088,0.113423249576877,3.53671738742444));
#23343=CARTESIAN_POINT('Ctrl Pts',(13.5650824502587,0.319731677430589,3.64606883846313));
#23344=CARTESIAN_POINT('Ctrl Pts',(13.5886965664085,0.449414183027706,3.84024235619866));
#23345=CARTESIAN_POINT('Ctrl Pts',(13.6123106825584,0.471391451138094,4.07270290539818));
#23346=CARTESIAN_POINT('Ctrl Pts',(13.6359247987083,0.380396476467901,4.28773969720951));
#23347=CARTESIAN_POINT('Ctrl Pts',(13.6595389148581,0.198236838143636,4.43381766753122));
#23348=CARTESIAN_POINT('Ctrl Pts',(13.683153031008,-0.0314316384354341,
4.47592821387755));
#23349=CARTESIAN_POINT('Ctrl Pts',(13.7067671471579,-0.253567304057185,
4.40397925067086));
#23350=CARTESIAN_POINT('Ctrl Pts',(13.7303812633077,-0.414933800093862,
4.23521384780468));
#23351=CARTESIAN_POINT('Ctrl Pts',(13.7539953794576,-0.476858522443512,
4.01007780890896));
#23352=CARTESIAN_POINT('Ctrl Pts',(13.7776094956075,-0.424500780316106,
3.78252655295316));
#23353=CARTESIAN_POINT('Ctrl Pts',(13.8012236117573,-0.270408471092428,
3.60709432248837));
#23354=CARTESIAN_POINT('Ctrl Pts',(13.8248377279072,-0.0515108893666192,
3.52582467278856));
#23355=CARTESIAN_POINT('Ctrl Pts',(13.8484518440571,0.179731635580624,3.55819444114981));
#23356=CARTESIAN_POINT('Ctrl Pts',(13.8720659602069,0.367900222888263,3.69644598724744));
#23357=CARTESIAN_POINT('Ctrl Pts',(13.8956800763568,0.467898960702838,3.90744636564338));
#23358=CARTESIAN_POINT('Ctrl Pts',(13.9192941925067,0.455762455382048,4.14062786681004));
#23359=CARTESIAN_POINT('Ctrl Pts',(13.9429083086565,0.33439930491234,4.34010692073752));
#23360=CARTESIAN_POINT('Ctrl Pts',(13.9665224248064,0.132895033153719,4.45807698351094));
#23361=CARTESIAN_POINT('Ctrl Pts',(13.9901365409563,-0.100458458427467,
4.46626570835715));
#23362=CARTESIAN_POINT('Ctrl Pts',(14.0137506571061,-0.309736381121202,
4.36271061036225));
#23363=CARTESIAN_POINT('Ctrl Pts',(14.037364773256,-0.444783823899526,4.1722293896428));
#23364=CARTESIAN_POINT('Ctrl Pts',(14.0609788894059,-0.473235726989685,
3.94047219674841));
#23365=CARTESIAN_POINT('Ctrl Pts',(14.0845930055557,-0.388273393752801,
3.72298125629644));
#23366=CARTESIAN_POINT('Ctrl Pts',(14.1082071217056,-0.210258638800633,
3.5718797861942));
#23367=CARTESIAN_POINT('Ctrl Pts',(14.1318212378555,0.0181460626216094,
3.52338030562014));
#23368=CARTESIAN_POINT('Ctrl Pts',(14.1554353540053,0.242201933815703,3.58910605271512));
#23369=CARTESIAN_POINT('Ctrl Pts',(14.1790494701552,0.40821242552128,3.75330539464867));
#23370=CARTESIAN_POINT('Ctrl Pts',(14.2026635863051,0.476391967745912,3.97662681607925));
#23371=CARTESIAN_POINT('Ctrl Pts',(14.2262777024549,0.430400858574612,4.20554978374509));
#23372=CARTESIAN_POINT('Ctrl Pts',(14.2498918186048,0.28126118747995,4.38521131483484));
#23373=CARTESIAN_POINT('Ctrl Pts',(14.2735059347547,0.0647153148514563,
4.47255427273816));
#23374=CARTESIAN_POINT('Ctrl Pts',(14.2971200509045,-0.167340033486385,
4.44664630956965));
#23375=CARTESIAN_POINT('Ctrl Pts',(14.3207341670544,-0.359291177888639,
4.31369644905674));
#23376=CARTESIAN_POINT('Ctrl Pts',(14.3443482832043,-0.465135690362464,
4.10556705078029));
#23377=CARTESIAN_POINT('Ctrl Pts',(14.3679623993541,-0.459507196674052,
3.87213777389641));
#23378=CARTESIAN_POINT('Ctrl Pts',(14.391576515504,-0.343754604517688,3.66935156959044));
#23379=CARTESIAN_POINT('Ctrl Pts',(14.4151906316539,-0.145618828396573,
3.5458075633877));
#23380=CARTESIAN_POINT('Ctrl Pts',(14.4388047478037,0.0874155136516737,
3.53111393640625));
#23381=CARTESIAN_POINT('Ctrl Pts',(14.4624188639536,0.299500119324396,3.6287921186396));
#23382=CARTESIAN_POINT('Ctrl Pts',(14.4860329801035,0.439807436479269,3.81543285374444));
#23383=CARTESIAN_POINT('Ctrl Pts',(14.5096470962533,0.474711839833821,4.04630639028407));
#23384=CARTESIAN_POINT('Ctrl Pts',(14.5332612124032,0.395848246141948,4.26608227803701));
#23385=CARTESIAN_POINT('Ctrl Pts',(14.5568753285531,0.22211686462983,4.42208969557108));
#23386=CARTESIAN_POINT('Ctrl Pts',(14.5804894447029,-0.00484636972403486,
4.47694037924932));
#23387=CARTESIAN_POINT('Ctrl Pts',(14.6041035608528,-0.230648137830783,
4.41748898090375));
#23388=CARTESIAN_POINT('Ctrl Pts',(14.6277176770027,-0.401173474098533,
4.25798344198848));
#23389=CARTESIAN_POINT('Ctrl Pts',(14.6513317931525,-0.475554794568933,
4.03665037532088));
#23390=CARTESIAN_POINT('Ctrl Pts',(14.6749459093024,-0.435966098077497,
3.80653379100725));
#23391=CARTESIAN_POINT('Ctrl Pts',(14.6985600254523,-0.291895091157815,
3.62278273060111));
#23392=CARTESIAN_POINT('Ctrl Pts',(14.7221741416021,-0.077869393911261,
3.52943441444639));
#23393=CARTESIAN_POINT('Ctrl Pts',(14.745788257752,0.15481824619589,3.54886041727207));
#23394=CARTESIAN_POINT('Ctrl Pts',(14.7694023739019,0.350402614714918,3.67640516027076));
#23395=CARTESIAN_POINT('Ctrl Pts',(14.7930164900517,0.462010559799276,3.88150166218328));
#23396=CARTESIAN_POINT('Ctrl Pts',(14.8166306062016,0.46289445276163,4.11499710940664));
#23397=CARTESIAN_POINT('Ctrl Pts',(14.8402447223515,0.352842479009638,4.32093271222338));
#23398=CARTESIAN_POINT('Ctrl Pts',(14.8638588385013,0.158229324796562,4.44995452773844));
#23399=CARTESIAN_POINT('Ctrl Pts',(14.8874729546512,-0.07430453695484,4.47114166986524));
#23400=CARTESIAN_POINT('Ctrl Pts',(14.9110870708011,-0.289030909828268,
4.37941629936134));
#23401=CARTESIAN_POINT('Ctrl Pts',(14.9347011869509,-0.434488776346555,
4.1967614535327));
#23402=CARTESIAN_POINT('Ctrl Pts',(14.9583153031008,-0.475818891632353,
3.96695075151007));
#23403=CARTESIAN_POINT('Ctrl Pts',(14.9819294192507,-0.403114615376237,
3.74506182641449));
#23404=CARTESIAN_POINT('Ctrl Pts',(15.0055435354005,-0.233803473716137,
3.58426783839933));
#23405=CARTESIAN_POINT('Ctrl Pts',(15.0291576515504,-0.00845486712728951,
3.5231129029393));
#23406=CARTESIAN_POINT('Ctrl Pts',(15.0527717677003,0.218908482701231,3.57623459158499));
#23407=CARTESIAN_POINT('Ctrl Pts',(15.0763858838501,0.393827738276586,3.73094220011788));
#23408=CARTESIAN_POINT('Ctrl Pts',(15.09212862795,0.447465415643859,3.87702813324079));
#23409=CARTESIAN_POINT('Ctrl Pts',(15.1,0.455362409197302,3.95209810113337));
#23410=CARTESIAN_POINT('',(15.1,0.455362409197302,3.95209810113338));
#23411=CARTESIAN_POINT('Ctrl Pts',(15.1,0.455362409197302,3.95209810113337));
#23412=CARTESIAN_POINT('Ctrl Pts',(15.1,0.461198486074795,3.93070554260298));
#23413=CARTESIAN_POINT('Ctrl Pts',(15.1,0.46535922191849,3.9089149747703));
#23414=CARTESIAN_POINT('Ctrl Pts',(15.1,0.467933495509747,3.88694781877637));
#23415=CARTESIAN_POINT('Ctrl Pts',(15.1,0.470556099470815,3.86456824322593));
#23416=CARTESIAN_POINT('Ctrl Pts',(15.1,0.471533159003394,3.84200460508655));
#23417=CARTESIAN_POINT('Ctrl Pts',(15.1,0.470938919222204,3.8194389967166));
#23418=CARTESIAN_POINT('Ctrl Pts',(15.1,0.470570970565677,3.80546654730098));
#23419=CARTESIAN_POINT('Ctrl Pts',(15.1,0.469600118414825,3.7914923521806));
#23420=CARTESIAN_POINT('Ctrl Pts',(15.1,0.468037922355437,3.77755218535593));
#23421=CARTESIAN_POINT('Ctrl Pts',(15.1,0.467305764617198,3.77101881782393));
#23422=CARTESIAN_POINT('Ctrl Pts',(15.1,0.466444065557791,3.76449770946228));
#23423=CARTESIAN_POINT('Ctrl Pts',(15.1,0.465455885979624,3.7580011302485));
#23424=CARTESIAN_POINT('Ctrl Pts',(15.1,0.462059294618766,3.73567095330476));
#23425=CARTESIAN_POINT('Ctrl Pts',(15.1,0.45716703427379,3.71360451488159));
#23426=CARTESIAN_POINT('Ctrl Pts',(15.1,0.450855318277529,3.69195899424001));
#23427=CARTESIAN_POINT('Ctrl Pts',(15.1,0.444011336009419,3.66848810937402));
#23428=CARTESIAN_POINT('Ctrl Pts',(15.1,0.435499564516811,3.64551127788848));
#23429=CARTESIAN_POINT('Ctrl Pts',(15.1,0.425460105602329,3.62314791088594));
#23430=CARTESIAN_POINT('Ctrl Pts',(15.1,0.421555366121865,3.61444992000866));
#23431=CARTESIAN_POINT('Ctrl Pts',(15.1,0.417417266816347,3.60584160863805));
#23432=CARTESIAN_POINT('Ctrl Pts',(15.1,0.413065612826793,3.5973533346642));
#23433=CARTESIAN_POINT('Ctrl Pts',(15.1,0.400188909388694,3.57223622128044));
#23434=CARTESIAN_POINT('Ctrl Pts',(15.1,0.385429835973237,3.54813135585314));
#23435=CARTESIAN_POINT('Ctrl Pts',(15.1,0.369010648251791,3.52520488756047));
#23436=CARTESIAN_POINT('Ctrl Pts',(15.1,0.352591460530346,3.50227841926781));
#23437=CARTESIAN_POINT('Ctrl Pts',(15.1,0.334512091502091,3.48052876229398));
#23438=CARTESIAN_POINT('Ctrl Pts',(15.1,0.31493781544227,3.46010549098216));
#23439=CARTESIAN_POINT('Ctrl Pts',(14.8800042915148,-1.01702808208336E-5,
4.45785711824254));
#23440=CARTESIAN_POINT('Ctrl Pts',(14.8824938458936,-0.0238866377941533,
4.45787702641871));
#23441=CARTESIAN_POINT('Ctrl Pts',(14.8849834002724,-0.0477600743578134,
4.45604121816599));
#23442=CARTESIAN_POINT('Ctrl Pts',(14.8874729546512,-0.0713366221418418,
4.45232291776013));
#23443=CARTESIAN_POINT('Ctrl Pts',(14.8953443267012,-0.145879994579315,
4.44056654636394));
#23444=CARTESIAN_POINT('Ctrl Pts',(14.9032156987511,-0.217455452203791,
4.40999142286264));
#23445=CARTESIAN_POINT('Ctrl Pts',(14.9110870708011,-0.277486158769077,
4.36426138680722));
#23446=CARTESIAN_POINT('Ctrl Pts',(14.918958442851,-0.337516865334364,4.31853135075179));
#23447=CARTESIAN_POINT('Ctrl Pts',(14.926829814901,-0.38600282084046,4.25764640214225));
#23448=CARTESIAN_POINT('Ctrl Pts',(14.9347011869509,-0.417134151141141,
4.18890214416703));
#23449=CARTESIAN_POINT('Ctrl Pts',(14.9425725590009,-0.448265481441821,
4.12015788619182));
#23450=CARTESIAN_POINT('Ctrl Pts',(14.9504439310508,-0.462042186537087,
4.04355431885095));
#23451=CARTESIAN_POINT('Ctrl Pts',(14.9583153031008,-0.456813159708701,
3.96827104766458));
#23452=CARTESIAN_POINT('Ctrl Pts',(14.9661866751508,-0.451584132880315,
3.89298777647821));
#23453=CARTESIAN_POINT('Ctrl Pts',(14.9740580472007,-0.427349374128277,
3.81902480144635));
#23454=CARTESIAN_POINT('Ctrl Pts',(14.9819294192507,-0.387013471142241,
3.7552443159279));
#23455=CARTESIAN_POINT('Ctrl Pts',(14.9898007913006,-0.346677568156205,
3.69146383040944));
#23456=CARTESIAN_POINT('Ctrl Pts',(14.9976721633506,-0.290240520936171,
3.63786583440439));
#23457=CARTESIAN_POINT('Ctrl Pts',(15.0055435354005,-0.224463896228013,
3.60087434715852));
#23458=CARTESIAN_POINT('Ctrl Pts',(15.0134149074505,-0.158687271519854,
3.56388285991266));
#23459=CARTESIAN_POINT('Ctrl Pts',(15.0212862795004,-0.0835710693235713,
3.54349788142598));
#23460=CARTESIAN_POINT('Ctrl Pts',(15.0291576515504,-0.00811907658734153,
3.54215900695692));
#23461=CARTESIAN_POINT('Ctrl Pts',(15.0370290236004,0.067332916148885,3.54082013248786));
#23462=CARTESIAN_POINT('Ctrl Pts',(15.0449003956503,0.143120699425059,3.55852736203643));
#23463=CARTESIAN_POINT('Ctrl Pts',(15.0527717677003,0.210167800325704,3.59316557823286));
#23464=CARTESIAN_POINT('Ctrl Pts',(15.0606431397502,0.27721490122635,3.62780379442929));
#23465=CARTESIAN_POINT('Ctrl Pts',(15.0685145118002,0.335521319751467,3.67937299727358));
#23466=CARTESIAN_POINT('Ctrl Pts',(15.0763858838501,0.378083948355844,3.74167908197646));
#23467=CARTESIAN_POINT('Ctrl Pts',(15.0842572559001,0.420646576960222,3.80398516667934));
#23468=CARTESIAN_POINT('Ctrl Pts',(15.09212862795,0.447465415643859,3.87702813324079));
#23469=CARTESIAN_POINT('Ctrl Pts',(15.1,0.455362409197302,3.95209810113337));
#23470=CARTESIAN_POINT('Ctrl Pts',(12.5,0.310062960217722,4.54266560670548));
#23471=CARTESIAN_POINT('Ctrl Pts',(12.5,0.283442099593322,4.54921865641189));
#23472=CARTESIAN_POINT('Ctrl Pts',(12.5,0.256466577744696,4.55390832200786));
#23473=CARTESIAN_POINT('Ctrl Pts',(12.5,0.229324391633413,4.55669460918752));
#23474=CARTESIAN_POINT('Ctrl Pts',(12.5,0.202804350211112,4.55941702996513));
#23475=CARTESIAN_POINT('Ctrl Pts',(12.5,0.176124140498118,4.56032157710196));
#23476=CARTESIAN_POINT('Ctrl Pts',(12.5,0.149491279718871,4.55933465732487));
#23477=CARTESIAN_POINT('Ctrl Pts',(12.5,0.131604301980395,4.55867182909064));
#23478=CARTESIAN_POINT('Ctrl Pts',(12.5,0.113739373486447,4.5571550748263));
#23479=CARTESIAN_POINT('Ctrl Pts',(12.5,0.0959711573489174,4.5547553284502));
#23480=CARTESIAN_POINT('Ctrl Pts',(12.5,0.0885102514788159,4.55374767063663));
#23481=CARTESIAN_POINT('Ctrl Pts',(12.5,0.0810658284660142,4.55258395860043));
#23482=CARTESIAN_POINT('Ctrl Pts',(12.5,0.0736590895785168,4.55126509319275));
#23483=CARTESIAN_POINT('Ctrl Pts',(12.5,0.0532014046082737,4.54762233847462));
#23484=CARTESIAN_POINT('Ctrl Pts',(12.5,0.0329999615976937,4.54279338637244));
#23485=CARTESIAN_POINT('Ctrl Pts',(12.5,0.0131662989716721,4.53674486487483));
#23486=CARTESIAN_POINT('Ctrl Pts',(12.5,-0.00550403753485725,4.53105111411095));
#23487=CARTESIAN_POINT('Ctrl Pts',(12.5,-0.0238485481480196,4.52427602479051));
#23488=CARTESIAN_POINT('Ctrl Pts',(12.5,-0.0417515783368052,4.51643454453567));
#23489=CARTESIAN_POINT('Ctrl Pts',(12.5,-0.0500477299146631,4.51280085190917));
#23490=CARTESIAN_POINT('Ctrl Pts',(12.5,-0.058248775177811,4.50893813195896));
#23491=CARTESIAN_POINT('Ctrl Pts',(12.5,-0.0663415323109863,4.50484786558969));
#23492=CARTESIAN_POINT('Ctrl Pts',(12.5,-0.0727048112135971,4.50163171746301));
#23493=CARTESIAN_POINT('Ctrl Pts',(12.5,-0.0789919703630761,4.49827952355299));
#23494=CARTESIAN_POINT('Ctrl Pts',(12.5,-0.085197598682301,4.4947927546146));
#23495=CARTESIAN_POINT('Ctrl Pts',(12.5,-0.104491803581693,4.48395188067351));
#23496=CARTESIAN_POINT('Ctrl Pts',(12.5,-0.123002674071495,4.47180959856144));
#23497=CARTESIAN_POINT('Ctrl Pts',(12.5,-0.140547257611399,4.45840101528927));
#23498=CARTESIAN_POINT('Ctrl Pts',(12.5,-0.156644205929787,4.44609879839914));
#23499=CARTESIAN_POINT('Ctrl Pts',(12.5,-0.17192740174072,4.43272977950413));
#23500=CARTESIAN_POINT('Ctrl Pts',(12.5,-0.186217277007305,4.41832740439832));
#23501=CARTESIAN_POINT('Origin',(15.1,0.,4.));
#23502=CARTESIAN_POINT('',(15.1,-1.16619037896906,2.5));
#23503=CARTESIAN_POINT('',(15.1,1.16619037896906,2.5));
#23504=CARTESIAN_POINT('',(15.1,1.25,2.5));
#23505=CARTESIAN_POINT('Origin',(15.1,0.,4.));
#23506=CARTESIAN_POINT('Origin',(15.1,0.,4.));
#23507=CARTESIAN_POINT('',(15.1,2.75545529808154E-17,5.725));
#23508=CARTESIAN_POINT('Origin',(15.1,0.,5.5));
#23509=CARTESIAN_POINT('',(15.1,1.5,4.225));
#23510=CARTESIAN_POINT('Origin',(15.1,1.5,4.));
#23511=CARTESIAN_POINT('',(15.1,-1.5,4.225));
#23512=CARTESIAN_POINT('Origin',(15.1,-1.5,4.));
#23513=CARTESIAN_POINT('Origin',(14.4,-1.5,4.));
#23514=CARTESIAN_POINT('',(14.5,-1.5,4.225));
#23515=CARTESIAN_POINT('Origin',(14.5,-1.5,4.));
#23516=CARTESIAN_POINT('',(14.4,-1.5,4.225));
#23517=CARTESIAN_POINT('Origin',(14.4,1.5,4.));
#23518=CARTESIAN_POINT('',(14.5,1.5,4.225));
#23519=CARTESIAN_POINT('Origin',(14.5,1.5,4.));
#23520=CARTESIAN_POINT('',(14.4,1.5,4.225));
#23521=CARTESIAN_POINT('Origin',(14.4,0.,5.5));
#23522=CARTESIAN_POINT('',(14.5,-2.75545529808154E-17,5.725));
#23523=CARTESIAN_POINT('Origin',(14.5,0.,5.5));
#23524=CARTESIAN_POINT('',(14.4,-2.75545529808154E-17,5.725));
#23525=CARTESIAN_POINT('Origin',(14.4,2.5,2.5));
#23526=CARTESIAN_POINT('',(14.5,1.16619037896906,2.5));
#23527=CARTESIAN_POINT('',(14.5,-1.16619037896906,2.5));
#23528=CARTESIAN_POINT('',(14.5,1.25,2.5));
#23529=CARTESIAN_POINT('',(14.5,1.16619037896906,2.5));
#23530=CARTESIAN_POINT('',(14.5,-1.16619037896906,2.5));
#23531=CARTESIAN_POINT('Origin',(14.5,0.,4.));
#23532=CARTESIAN_POINT('Origin',(14.5,0.,4.));
#23533=CARTESIAN_POINT('',(14.5,-1.34711147906209E-16,5.1));
#23534=CARTESIAN_POINT('Origin',(14.5,0.,4.));
#23535=CARTESIAN_POINT('Origin',(14.5,0.,4.));
#23536=CARTESIAN_POINT('Origin',(12.5,0.,4.));
#23537=CARTESIAN_POINT('Origin',(12.5,0.,4.));
#23538=CARTESIAN_POINT('',(12.5,-1.34711147906209E-16,5.1));
#23539=CARTESIAN_POINT('',(12.5,-1.34711147906209E-16,5.1));
#23540=CARTESIAN_POINT('Origin',(12.5,0.,4.));
#23541=CARTESIAN_POINT('Origin',(12.5,0.,4.));
#23542=CARTESIAN_POINT('',(0.,0.,0.));
#23543=CARTESIAN_POINT('Origin',(0.3,0.4,0.));
#23544=CARTESIAN_POINT('',(-0.3,0.4,-3.67394039744206E-17));
#23545=CARTESIAN_POINT('Origin',(0.,0.4,0.));
#23546=CARTESIAN_POINT('Origin',(0.,0.375,0.));
#23547=CARTESIAN_POINT('',(-0.35,0.35,-4.28626379701573E-17));
#23548=CARTESIAN_POINT('Origin',(0.,0.35,0.));
#23549=CARTESIAN_POINT('',(-0.325,0.375,-3.9801020972289E-17));
#23550=CARTESIAN_POINT('Origin',(0.,0.19,0.));
#23551=CARTESIAN_POINT('',(-0.35,0.03,-4.28626379701574E-17));
#23552=CARTESIAN_POINT('Origin',(0.,0.03,0.));
#23553=CARTESIAN_POINT('',(-0.35,0.19,-4.28626379701574E-17));
#23554=CARTESIAN_POINT('Origin',(0.,0.0149999999999999,0.));
#23555=CARTESIAN_POINT('',(-0.32,-3.29597460435593E-17,-3.91886975727153E-17));
#23556=CARTESIAN_POINT('Origin',(0.,0.,0.));
#23557=CARTESIAN_POINT('',(-0.335,0.0149999999999999,-4.10256677714363E-17));
#23558=CARTESIAN_POINT('Origin',(0.22,0.,0.));
#23559=CARTESIAN_POINT('',(-0.22,-6.93889390390723E-18,-2.69422295812418E-17));
#23560=CARTESIAN_POINT('Origin',(0.,0.,0.));
#23561=CARTESIAN_POINT('Origin',(0.,-0.02,0.));
#23562=CARTESIAN_POINT('',(-0.1954,-0.0492,2.39295984553393E-17));
#23563=CARTESIAN_POINT('Origin',(0.,-0.0492,0.));
#23564=CARTESIAN_POINT('',(-0.21,-0.02,-2.57175827820944E-17));
#23565=CARTESIAN_POINT('Origin',(0.,-0.8,0.));
#23566=CARTESIAN_POINT('',(-0.1954,-1.5646,2.39295984553393E-17));
#23567=CARTESIAN_POINT('Origin',(0.,-1.5646,0.));
#23568=CARTESIAN_POINT('',(-0.1954,-0.8,-2.39295984553393E-17));
#23569=CARTESIAN_POINT('Origin',(0.,-1.58,0.));
#23570=CARTESIAN_POINT('',(-0.16,-1.6,-1.95943487863577E-17));
#23571=CARTESIAN_POINT('Origin',(0.,-1.6,0.));
#23572=CARTESIAN_POINT('',(-0.18,-1.58,-2.20436423846524E-17));
#23573=CARTESIAN_POINT('Origin',(0.,-1.6,0.));
#23574=CARTESIAN_POINT('Origin',(0.0866025403784439,-0.4,-0.15));
#23575=CARTESIAN_POINT('',(0.173205080756888,-0.4,0.));
#23576=CARTESIAN_POINT('',(0.0866025403784439,-0.4,-0.15));
#23577=CARTESIAN_POINT('',(0.173205080756888,-0.4,0.));
#23578=CARTESIAN_POINT('',(0.0866025403784439,-0.64,-0.15));
#23579=CARTESIAN_POINT('',(0.0866025403784439,-0.4,-0.15));
#23580=CARTESIAN_POINT('',(0.173205080756888,-0.64,0.));
#23581=CARTESIAN_POINT('',(0.173205080756888,-0.64,0.));
#23582=CARTESIAN_POINT('',(0.173205080756888,-0.4,0.));
#23583=CARTESIAN_POINT('Origin',(-0.0866025403784438,-0.4,-0.15));
#23584=CARTESIAN_POINT('',(-0.0866025403784438,-0.4,-0.15));
#23585=CARTESIAN_POINT('',(0.0866025403784439,-0.4,-0.15));
#23586=CARTESIAN_POINT('',(-0.0866025403784438,-0.64,-0.15));
#23587=CARTESIAN_POINT('',(-0.0866025403784438,-0.4,-0.15));
#23588=CARTESIAN_POINT('',(0.0866025403784439,-0.64,-0.15));
#23589=CARTESIAN_POINT('Origin',(-0.173205080756888,-0.4,-2.77555756156289E-17));
#23590=CARTESIAN_POINT('',(-0.173205080756888,-0.4,-2.12115047744981E-17));
#23591=CARTESIAN_POINT('',(-0.0866025403784438,-0.4,-0.15));
#23592=CARTESIAN_POINT('',(-0.173205080756888,-0.64,-2.77555756156289E-17));
#23593=CARTESIAN_POINT('',(-0.173205080756888,-0.4,-2.12115047744981E-17));
#23594=CARTESIAN_POINT('',(-0.0866025403784438,-0.64,-0.15));
#23595=CARTESIAN_POINT('Origin',(-0.0866025403784439,-0.4,0.15));
#23596=CARTESIAN_POINT('',(-0.0866025403784439,-0.4,0.15));
#23597=CARTESIAN_POINT('',(-0.173205080756888,-0.4,-2.12115047744981E-17));
#23598=CARTESIAN_POINT('',(-0.0866025403784439,-0.64,0.15));
#23599=CARTESIAN_POINT('',(-0.0866025403784439,-0.4,0.15));
#23600=CARTESIAN_POINT('',(-0.173205080756888,-0.64,-2.12115047744981E-17));
#23601=CARTESIAN_POINT('Origin',(0.0866025403784439,-0.4,0.15));
#23602=CARTESIAN_POINT('',(0.0866025403784439,-0.4,0.15));
#23603=CARTESIAN_POINT('',(-0.0866025403784439,-0.4,0.15));
#23604=CARTESIAN_POINT('',(0.0866025403784439,-0.64,0.15));
#23605=CARTESIAN_POINT('',(0.0866025403784439,-0.4,0.15));
#23606=CARTESIAN_POINT('',(-0.0866025403784439,-0.64,0.15));
#23607=CARTESIAN_POINT('Origin',(0.173205080756888,-0.4,0.));
#23608=CARTESIAN_POINT('',(0.0866025403784439,-0.4,0.15));
#23609=CARTESIAN_POINT('',(0.0866025403784439,-0.64,0.15));
#23610=CARTESIAN_POINT('Origin',(0.,-0.4,-2.77555756156289E-17));
#23611=CARTESIAN_POINT('Origin',(0.,-0.64,-2.77555756156289E-17));
#23612=CARTESIAN_POINT('',(0.,0.,0.));
#23613=CARTESIAN_POINT('Origin',(0.375,0.5,0.));
#23614=CARTESIAN_POINT('',(-0.375,0.5,-4.59242549680257E-17));
#23615=CARTESIAN_POINT('Origin',(0.,0.5,0.));
#23616=CARTESIAN_POINT('Origin',(0.,0.475,0.));
#23617=CARTESIAN_POINT('',(-0.425,0.45,-5.20474889637625E-17));
#23618=CARTESIAN_POINT('Origin',(0.,0.45,0.));
#23619=CARTESIAN_POINT('',(-0.4,0.475,-4.89858719658941E-17));
#23620=CARTESIAN_POINT('Origin',(0.,0.24,0.));
#23621=CARTESIAN_POINT('',(-0.425,0.0299999999999998,-5.20474889637625E-17));
#23622=CARTESIAN_POINT('Origin',(0.,0.0299999999999998,0.));
#23623=CARTESIAN_POINT('',(-0.425,0.24,-5.20474889637625E-17));
#23624=CARTESIAN_POINT('Origin',(0.,0.0150000000000001,0.));
#23625=CARTESIAN_POINT('',(-0.395,4.85722573273506E-17,-4.83735485663204E-17));
#23626=CARTESIAN_POINT('Origin',(0.,0.,0.));
#23627=CARTESIAN_POINT('',(-0.41,0.0150000000000001,-5.02105187650415E-17));
#23628=CARTESIAN_POINT('Origin',(0.27,0.,0.));
#23629=CARTESIAN_POINT('',(-0.27,0.,-3.30654635769785E-17));
#23630=CARTESIAN_POINT('Origin',(0.,0.,0.));
#23631=CARTESIAN_POINT('Origin',(0.,-0.02,0.));
#23632=CARTESIAN_POINT('',(-0.24505,-0.0498999999999999,3.00099698131059E-17));
#23633=CARTESIAN_POINT('Origin',(0.,-0.0498999999999999,0.));
#23634=CARTESIAN_POINT('',(-0.26,-0.02,-3.18408167778312E-17));
#23635=CARTESIAN_POINT('Origin',(0.,-0.995,0.));
#23636=CARTESIAN_POINT('',(-0.24505,-1.95495,3.00099698131059E-17));
#23637=CARTESIAN_POINT('Origin',(0.,-1.95495,0.));
#23638=CARTESIAN_POINT('',(-0.24505,-0.995,-3.00099698131059E-17));
#23639=CARTESIAN_POINT('Origin',(0.,-1.975,0.));
#23640=CARTESIAN_POINT('',(-0.2,-2.,-2.44929359829471E-17));
#23641=CARTESIAN_POINT('Origin',(0.,-2.,0.));
#23642=CARTESIAN_POINT('',(-0.225,-1.975,-2.75545529808154E-17));
#23643=CARTESIAN_POINT('Origin',(0.,-2.,0.));
#23644=CARTESIAN_POINT('Origin',(0.115470053837925,-0.5,-0.2));
#23645=CARTESIAN_POINT('',(0.23094010767585,-0.5,0.));
#23646=CARTESIAN_POINT('',(0.115470053837925,-0.5,-0.2));
#23647=CARTESIAN_POINT('',(0.23094010767585,-0.5,0.));
#23648=CARTESIAN_POINT('',(0.115470053837925,-0.8,-0.2));
#23649=CARTESIAN_POINT('',(0.115470053837925,-0.5,-0.2));
#23650=CARTESIAN_POINT('',(0.23094010767585,-0.8,0.));
#23651=CARTESIAN_POINT('',(0.23094010767585,-0.8,0.));
#23652=CARTESIAN_POINT('',(0.23094010767585,-0.5,0.));
#23653=CARTESIAN_POINT('Origin',(-0.115470053837925,-0.5,-0.2));
#23654=CARTESIAN_POINT('',(-0.115470053837925,-0.5,-0.2));
#23655=CARTESIAN_POINT('',(0.115470053837925,-0.5,-0.2));
#23656=CARTESIAN_POINT('',(-0.115470053837925,-0.8,-0.2));
#23657=CARTESIAN_POINT('',(-0.115470053837925,-0.5,-0.2));
#23658=CARTESIAN_POINT('',(0.115470053837925,-0.8,-0.2));
#23659=CARTESIAN_POINT('Origin',(-0.23094010767585,-0.5,-2.77555756156289E-17));
#23660=CARTESIAN_POINT('',(-0.23094010767585,-0.5,-2.82820063659975E-17));
#23661=CARTESIAN_POINT('',(-0.115470053837925,-0.5,-0.2));
#23662=CARTESIAN_POINT('',(-0.23094010767585,-0.8,-2.77555756156289E-17));
#23663=CARTESIAN_POINT('',(-0.23094010767585,-0.5,-2.82820063659975E-17));
#23664=CARTESIAN_POINT('',(-0.115470053837925,-0.8,-0.2));
#23665=CARTESIAN_POINT('Origin',(-0.115470053837925,-0.5,0.2));
#23666=CARTESIAN_POINT('',(-0.115470053837925,-0.5,0.2));
#23667=CARTESIAN_POINT('',(-0.23094010767585,-0.5,-2.82820063659975E-17));
#23668=CARTESIAN_POINT('',(-0.115470053837925,-0.8,0.2));
#23669=CARTESIAN_POINT('',(-0.115470053837925,-0.5,0.2));
#23670=CARTESIAN_POINT('',(-0.23094010767585,-0.8,-2.82820063659975E-17));
#23671=CARTESIAN_POINT('Origin',(0.115470053837925,-0.5,0.2));
#23672=CARTESIAN_POINT('',(0.115470053837925,-0.5,0.2));
#23673=CARTESIAN_POINT('',(-0.115470053837925,-0.5,0.2));
#23674=CARTESIAN_POINT('',(0.115470053837925,-0.8,0.2));
#23675=CARTESIAN_POINT('',(0.115470053837925,-0.5,0.2));
#23676=CARTESIAN_POINT('',(-0.115470053837925,-0.8,0.2));
#23677=CARTESIAN_POINT('Origin',(0.23094010767585,-0.5,0.));
#23678=CARTESIAN_POINT('',(0.115470053837925,-0.5,0.2));
#23679=CARTESIAN_POINT('',(0.115470053837925,-0.8,0.2));
#23680=CARTESIAN_POINT('Origin',(0.,-0.5,0.));
#23681=CARTESIAN_POINT('Origin',(0.,-0.8,0.));
#23682=CARTESIAN_POINT('',(0.,0.,0.));
#23683=CARTESIAN_POINT('',(0.,0.,0.));
#23684=CARTESIAN_POINT('',(0.,0.,0.));
#23685=CARTESIAN_POINT('',(13.5,-6.,2.8));
#23686=CARTESIAN_POINT('',(12.,-7.9,7.2));
#23687=CARTESIAN_POINT('',(12.,-7.9,7.3));
#23688=CARTESIAN_POINT('',(12.,-4.1,7.2));
#23689=CARTESIAN_POINT('',(12.,-4.1,7.3));
#23690=CARTESIAN_POINT('',(15.,-7.9,7.2));
#23691=CARTESIAN_POINT('',(15.,-7.9,7.3));
#23692=CARTESIAN_POINT('',(15.,-4.1,7.2));
#23693=CARTESIAN_POINT('',(15.,-4.1,7.3));
#23694=CARTESIAN_POINT('',(0.,0.,0.));
#23695=CARTESIAN_POINT('',(15.1,-1.5,4.));
#23696=CARTESIAN_POINT('',(15.1,1.5,4.));
#23697=CARTESIAN_POINT('',(15.1,0.,5.5));
#23698=CARTESIAN_POINT('',(12.5,-1.5,7.2));
#23699=CARTESIAN_POINT('',(12.5,1.5,7.2));
#23700=CARTESIAN_POINT('',(14.,-1.5,7.2));
#23701=CARTESIAN_POINT('',(14.,1.5,7.2));
#23702=CARTESIAN_POINT('',(0.,0.,0.));
#23703=CARTESIAN_POINT('',(0.,0.,0.));
#23704=CARTESIAN_POINT('Origin',(4.,0.,4.));
#23705=CARTESIAN_POINT('',(4.12884541125756,8.40637486662632E-6,4.59405635738975));
#23706=CARTESIAN_POINT('',(4.02115458874249,-9.26662433349265E-6,4.59413599269206));
#23707=CARTESIAN_POINT('',(4.,-7.27562663373442E-17,4.5941));
#23708=CARTESIAN_POINT('',(4.,0.254721014554615,3.46322028700965));
#23709=CARTESIAN_POINT('Ctrl Pts',(4.12884541125756,8.40637486662632E-6,
4.59405635738975));
#23710=CARTESIAN_POINT('Ctrl Pts',(4.12564700130467,0.0398130654959074,
4.59407663624518));
#23711=CARTESIAN_POINT('Ctrl Pts',(4.12244859135178,0.079613792300143,4.59013569217808));
#23712=CARTESIAN_POINT('Ctrl Pts',(4.11925018139889,0.118599576779877,4.58219388355888));
#23713=CARTESIAN_POINT('Ctrl Pts',(4.11129754205509,0.215535206692688,4.56244709042845));
#23714=CARTESIAN_POINT('Ctrl Pts',(4.10334490271129,0.30743256945264,4.51796551073728));
#23715=CARTESIAN_POINT('Ctrl Pts',(4.09539226336748,0.383054411795556,4.45418672179759));
#23716=CARTESIAN_POINT('Ctrl Pts',(4.08743962402367,0.458676254138472,4.3904079328579));
#23717=CARTESIAN_POINT('Ctrl Pts',(4.07948698467986,0.518022576064352,4.30733193466969));
#23718=CARTESIAN_POINT('Ctrl Pts',(4.07153434533606,0.553840407547632,4.21511760274296));
#23719=CARTESIAN_POINT('Ctrl Pts',(4.06358170599225,0.589658239030912,4.12290327081622));
#23720=CARTESIAN_POINT('Ctrl Pts',(4.05562906664845,0.601947580071592,4.02155060515096));
#23721=CARTESIAN_POINT('Ctrl Pts',(4.04767642730464,0.589200356533535,3.92344812692479));
#23722=CARTESIAN_POINT('Ctrl Pts',(4.03972378796084,0.576453132995478,3.82534564869861));
#23723=CARTESIAN_POINT('Ctrl Pts',(4.03177114861703,0.538669344878685,3.73049335791153));
#23724=CARTESIAN_POINT('Ctrl Pts',(4.02381850927322,0.480479105222089,3.65049437695417));
#23725=CARTESIAN_POINT('Ctrl Pts',(4.01587900618215,0.422384984811151,3.57062753914914));
#23726=CARTESIAN_POINT('Ctrl Pts',(4.00793950309107,0.343951772361455,3.50556498199611));
#23727=CARTESIAN_POINT('Ctrl Pts',(4.,0.254721014554615,3.46322028700965));
#23728=CARTESIAN_POINT('',(4.,0.254694598474614,4.53673594206822));
#23729=CARTESIAN_POINT('Origin',(4.,0.,4.));
#23730=CARTESIAN_POINT('Ctrl Pts',(3.99999999999998,0.254694598474614,4.53673594206822));
#23731=CARTESIAN_POINT('Ctrl Pts',(4.00705152958082,0.175425736340139,4.5743509952638));
#23732=CARTESIAN_POINT('Ctrl Pts',(4.01410305916165,0.0876996967667308,
4.59405101338575));
#23733=CARTESIAN_POINT('Ctrl Pts',(4.02115458874249,-9.26662433349265E-6,
4.59413599269206));
#23734=CARTESIAN_POINT('Origin',(4.,0.,4.));
#23735=CARTESIAN_POINT('',(4.42884541125756,-2.46302091461148E-6,4.59415045696459));
#23736=CARTESIAN_POINT('',(4.32115458874249,3.58587963140688E-6,4.59404994535016));
#23737=CARTESIAN_POINT('',(4.,-7.27562663373442E-17,4.5941));
#23738=CARTESIAN_POINT('Ctrl Pts',(4.42884541125756,-2.46302091461148E-6,
4.59415045696459));
#23739=CARTESIAN_POINT('Ctrl Pts',(4.42107867343035,0.0966117732708647,
4.59412799973471));
#23740=CARTESIAN_POINT('Ctrl Pts',(4.41331193560314,0.193236775309615,4.57009608476161));
#23741=CARTESIAN_POINT('Ctrl Pts',(4.40554519777592,0.278573173318151,4.52479781884576));
#23742=CARTESIAN_POINT('Ctrl Pts',(4.39759255843212,0.36595214906825,4.47841531183407));
#23743=CARTESIAN_POINT('Ctrl Pts',(4.38963991908831,0.441495654419193,4.40973622444741));
#23744=CARTESIAN_POINT('Ctrl Pts',(4.3816872797445,0.495967466205845,4.32715751007026));
#23745=CARTESIAN_POINT('Ctrl Pts',(4.3737346404007,0.550439277992498,4.24457879569311));
#23746=CARTESIAN_POINT('Ctrl Pts',(4.36578200105689,0.58383939621486,4.14810045432546));
#23747=CARTESIAN_POINT('Ctrl Pts',(4.35782936171309,0.59208420294366,4.04951827803692));
#23748=CARTESIAN_POINT('Ctrl Pts',(4.34987672236928,0.600329009672459,3.95093610174838));
#23749=CARTESIAN_POINT('Ctrl Pts',(4.34192408302547,0.583418504907695,3.85025009053894));
#23750=CARTESIAN_POINT('Ctrl Pts',(4.33397144368167,0.54342022548472,3.75977047903001));
#23751=CARTESIAN_POINT('Ctrl Pts',(4.32601880433786,0.503421946061746,3.66929086752108));
#23752=CARTESIAN_POINT('Ctrl Pts',(4.31806616499406,0.440335891980562,3.58901765571266));
#23753=CARTESIAN_POINT('Ctrl Pts',(4.31011352565025,0.361875197644003,3.52876534000234));
#23754=CARTESIAN_POINT('Ctrl Pts',(4.30216088630644,0.283414503307443,3.46851302429202));
#23755=CARTESIAN_POINT('Ctrl Pts',(4.29420824696263,0.189579168715509,3.4282816046798));
#23756=CARTESIAN_POINT('Ctrl Pts',(4.28625560761883,0.0918418319479975,
3.41298991457491));
#23757=CARTESIAN_POINT('Ctrl Pts',(4.27830296827502,-0.00589550481951406,
3.39769822447003));
#23758=CARTESIAN_POINT('Ctrl Pts',(4.27035032893122,-0.107534843762603,
3.4073462638725));
#23759=CARTESIAN_POINT('Ctrl Pts',(4.26239768958741,-0.200649373295791,
3.44075443909651));
#23760=CARTESIAN_POINT('Ctrl Pts',(4.25444505024361,-0.293763902828979,
3.47416261432052));
#23761=CARTESIAN_POINT('Ctrl Pts',(4.24649241089979,-0.378353622952266,
3.53133092536608));
#23762=CARTESIAN_POINT('Ctrl Pts',(4.23853977155599,-0.444076322467606,
3.60526974769923));
#23763=CARTESIAN_POINT('Ctrl Pts',(4.23058713221218,-0.509799021982947,
3.67920857003239));
#23764=CARTESIAN_POINT('Ctrl Pts',(4.22263449286838,-0.556654700890342,
3.76991790365313));
#23765=CARTESIAN_POINT('Ctrl Pts',(4.21468185352458,-0.578914549750806,
3.86630733464992));
#23766=CARTESIAN_POINT('Ctrl Pts',(4.20672921418077,-0.601174398611269,
3.96269676564671));
#23767=CARTESIAN_POINT('Ctrl Pts',(4.19877657483696,-0.598838417424802,
4.06476629401955));
#23768=CARTESIAN_POINT('Ctrl Pts',(4.19082393549315,-0.5721923335546,4.16003645884502));
#23769=CARTESIAN_POINT('Ctrl Pts',(4.18287129614934,-0.545546249684398,
4.25530662367048));
#23770=CARTESIAN_POINT('Ctrl Pts',(4.17491865680554,-0.494590063130461,
4.34377742494856));
#23771=CARTESIAN_POINT('Ctrl Pts',(4.16696601746173,-0.425553631634784,
4.41463223618795));
#23772=CARTESIAN_POINT('Ctrl Pts',(4.15901337811793,-0.356517200139107,
4.48548704742733));
#23773=CARTESIAN_POINT('Ctrl Pts',(4.15106073877413,-0.269400523701689,
4.53872586862801));
#23774=CARTESIAN_POINT('Ctrl Pts',(4.14310809943032,-0.174855236950146,
4.56783927594351));
#23775=CARTESIAN_POINT('Ctrl Pts',(4.1383538700394,-0.118334381217266,4.5852437891806));
#23776=CARTESIAN_POINT('Ctrl Pts',(4.13359964064848,-0.0591586432141876,
4.59402621418361));
#23777=CARTESIAN_POINT('Ctrl Pts',(4.12884541125756,8.40637486662632E-6,
4.59405635738975));
#23778=CARTESIAN_POINT('Ctrl Pts',(4.02115458874249,-9.26662433349265E-6,
4.59413599269206));
#23779=CARTESIAN_POINT('Ctrl Pts',(4.02205569850546,-0.0112175303500608,
4.59414685213492));
#23780=CARTESIAN_POINT('Ctrl Pts',(4.02295680826843,-0.0224255152200988,
4.5938373961197));
#23781=CARTESIAN_POINT('Ctrl Pts',(4.0238579180314,-0.0336155370699344,
4.59320407706013));
#23782=CARTESIAN_POINT('Ctrl Pts',(4.03181055737521,-0.132371772633995,
4.58761479340425));
#23783=CARTESIAN_POINT('Ctrl Pts',(4.03976319671902,-0.229728915328813,
4.55680066053817));
#23784=CARTESIAN_POINT('Ctrl Pts',(4.04771583606282,-0.31374319278985,4.50455967689729));
#23785=CARTESIAN_POINT('Ctrl Pts',(4.05566847540663,-0.397757470250888,
4.4523186932564));
#23786=CARTESIAN_POINT('Ctrl Pts',(4.06362111475043,-0.468428882478145,
4.37865085884071));
#23787=CARTESIAN_POINT('Ctrl Pts',(4.07157375409424,-0.517135915630147,
4.29254879227412));
#23788=CARTESIAN_POINT('Ctrl Pts',(4.07952639343804,-0.565842948782149,
4.20644672570752));
#23789=CARTESIAN_POINT('Ctrl Pts',(4.08747903278185,-0.592585602858896,
4.10791042699003));
#23790=CARTESIAN_POINT('Ctrl Pts',(4.09543167212566,-0.594084460855775,
4.00899459728238));
#23791=CARTESIAN_POINT('Ctrl Pts',(4.10338431146947,-0.595583318852653,
3.91007876757474));
#23792=CARTESIAN_POINT('Ctrl Pts',(4.11133695081327,-0.571838380769662,
3.81078340687695));
#23793=CARTESIAN_POINT('Ctrl Pts',(4.11928959015708,-0.525757920758293,
3.72324489380985));
#23794=CARTESIAN_POINT('Ctrl Pts',(4.12724222950088,-0.479677460746923,
3.63570638074275));
#23795=CARTESIAN_POINT('Ctrl Pts',(4.13519486884469,-0.411261478807175,
3.55992471530633));
#23796=CARTESIAN_POINT('Ctrl Pts',(4.1431475081885,-0.328872047298013,3.50516726345229));
#23797=CARTESIAN_POINT('Ctrl Pts',(4.1511001475323,-0.246482615788851,3.45040981159825));
#23798=CARTESIAN_POINT('Ctrl Pts',(4.15905278687611,-0.150119734710276,
3.41667657332659));
#23799=CARTESIAN_POINT('Ctrl Pts',(4.16700542621992,-0.0515665150750243,
3.40809082437526));
#23800=CARTESIAN_POINT('Ctrl Pts',(4.17495806556372,0.0469867045602276,
3.39950507542393));
#23801=CARTESIAN_POINT('Ctrl Pts',(4.18291070490753,0.147730262752155,3.41606681579293));
#23802=CARTESIAN_POINT('Ctrl Pts',(4.19086334425134,0.238347648045887,3.45575171487277));
#23803=CARTESIAN_POINT('Ctrl Pts',(4.19881598359514,0.32896503333962,3.49543661395261));
#23804=CARTESIAN_POINT('Ctrl Pts',(4.20676862293895,0.409456245735157,3.55824467174328));
#23805=CARTESIAN_POINT('Ctrl Pts',(4.21472126228276,0.469979735422806,3.63649644709345));
#23806=CARTESIAN_POINT('Ctrl Pts',(4.22267390162656,0.530503225110456,3.71474822244363));
#23807=CARTESIAN_POINT('Ctrl Pts',(4.23062654097037,0.571058992090217,3.80844371535332));
#23808=CARTESIAN_POINT('Ctrl Pts',(4.23857918031417,0.586688754827568,3.90612753493601));
#23809=CARTESIAN_POINT('Ctrl Pts',(4.24653181965798,0.602318517564919,4.0038113545187));
#23810=CARTESIAN_POINT('Ctrl Pts',(4.25448445900178,0.593022276059861,4.10548350077438));
#23811=CARTESIAN_POINT('Ctrl Pts',(4.26243709834559,0.559936509464549,4.19871308474845));
#23812=CARTESIAN_POINT('Ctrl Pts',(4.2703897376894,0.526850742869238,4.29194266872251));
#23813=CARTESIAN_POINT('Ctrl Pts',(4.27834237703321,0.469975451183674,4.37672969041494));
#23814=CARTESIAN_POINT('Ctrl Pts',(4.28629501637701,0.396264473279151,4.44270782630825));
#23815=CARTESIAN_POINT('Ctrl Pts',(4.29424765572082,0.322553495374627,4.50868596220156));
#23816=CARTESIAN_POINT('Ctrl Pts',(4.30220029506462,0.232006831251144,4.55585521229574));
#23817=CARTESIAN_POINT('Ctrl Pts',(4.31015293440843,0.135695012128791,4.57844846968215));
#23818=CARTESIAN_POINT('Ctrl Pts',(4.31382015251978,0.0912825306677821,
4.58886694826517));
#23819=CARTESIAN_POINT('Ctrl Pts',(4.31748737063114,0.0456441298716245,
4.59405951624442));
#23820=CARTESIAN_POINT('Ctrl Pts',(4.32115458874249,3.58587963140688E-6,
4.59404994535016));
#23821=CARTESIAN_POINT('Origin',(4.,0.,4.));
#23822=CARTESIAN_POINT('',(4.72884541125756,-4.67700812217808E-6,4.59405084457266));
#23823=CARTESIAN_POINT('',(4.62115458874249,3.7232086238465E-6,4.59414939806979));
#23824=CARTESIAN_POINT('',(4.,-7.27562663373442E-17,4.5941));
#23825=CARTESIAN_POINT('Ctrl Pts',(4.72884541125756,-4.67700812217808E-6,
4.59405084457266));
#23826=CARTESIAN_POINT('Ctrl Pts',(4.72446298489983,0.0545367878429411,
4.59403588702548));
#23827=CARTESIAN_POINT('Ctrl Pts',(4.7200805585421,0.10908225468116,4.58659074407712));
#23828=CARTESIAN_POINT('Ctrl Pts',(4.71569813218437,0.16154350694756,4.57176871113812));
#23829=CARTESIAN_POINT('Ctrl Pts',(4.70774549284056,0.256743148594298,4.54487167450041));
#23830=CARTESIAN_POINT('Ctrl Pts',(4.69979285349676,0.345079446524661,4.4936824501733));
#23831=CARTESIAN_POINT('Ctrl Pts',(4.69184021415295,0.415752085200636,4.42445961801412));
#23832=CARTESIAN_POINT('Ctrl Pts',(4.68388757480915,0.486424723876611,4.35523678585494));
#23833=CARTESIAN_POINT('Ctrl Pts',(4.67593493546534,0.539433703298198,4.26798034586369));
#23834=CARTESIAN_POINT('Ctrl Pts',(4.66798229612153,0.568297953762936,4.17335858623793));
#23835=CARTESIAN_POINT('Ctrl Pts',(4.66002965677773,0.597162204227674,4.07873682661218));
#23836=CARTESIAN_POINT('Ctrl Pts',(4.65207701743392,0.601881725735563,3.97674974735193));
#23837=CARTESIAN_POINT('Ctrl Pts',(4.64412437809011,0.581879492504365,3.87986665793328));
#23838=CARTESIAN_POINT('Ctrl Pts',(4.63617173874631,0.561877259273167,3.78298356851463));
#23839=CARTESIAN_POINT('Ctrl Pts',(4.6282190994025,0.517153271302883,3.69120446893757));
#23840=CARTESIAN_POINT('Ctrl Pts',(4.6202664600587,0.453175645250056,3.61575060413089));
#23841=CARTESIAN_POINT('Ctrl Pts',(4.61231382071489,0.389198019197228,3.5402967393242));
#23842=CARTESIAN_POINT('Ctrl Pts',(4.60436118137108,0.305966755061857,3.48116810928789));
#23843=CARTESIAN_POINT('Ctrl Pts',(4.59640854202727,0.213658008474022,3.4455939943611));
#23844=CARTESIAN_POINT('Ctrl Pts',(4.58845590268347,0.121349261886187,3.41001987943431));
#23845=CARTESIAN_POINT('Ctrl Pts',(4.58050326333966,0.0199630328458878,
3.39800027961704));
#23846=CARTESIAN_POINT('Ctrl Pts',(4.57255062399586,-0.0781048312986516,
3.41100475468789));
#23847=CARTESIAN_POINT('Ctrl Pts',(4.56459798465205,-0.17617269544319,3.42400922975875));
#23848=CARTESIAN_POINT('Ctrl Pts',(4.55664534530825,-0.270922194691968,
3.46203777971774));
#23849=CARTESIAN_POINT('Ctrl Pts',(4.54869270596444,-0.350768912290741,
3.52044089639904));
#23850=CARTESIAN_POINT('Ctrl Pts',(4.54074006662063,-0.430615629889515,
3.57884401308035));
#23851=CARTESIAN_POINT('Ctrl Pts',(4.53278742727683,-0.495559565838284,
3.65762169648397));
#23852=CARTESIAN_POINT('Ctrl Pts',(4.52483478793302,-0.537660439465301,
3.74714230187364));
#23853=CARTESIAN_POINT('Ctrl Pts',(4.51688214858921,-0.579761313092318,
3.8366629072633));
#23854=CARTESIAN_POINT('Ctrl Pts',(4.50892950924541,-0.599019124397585,
3.936926434639));
#23855=CARTESIAN_POINT('Ctrl Pts',(4.5009768699016,-0.593079343631488,4.03567430223551));
#23856=CARTESIAN_POINT('Ctrl Pts',(4.49302423055779,-0.587139562865391,
4.13442216983203));
#23857=CARTESIAN_POINT('Ctrl Pts',(4.48507159121399,-0.556002190027932,
4.23165437764937));
#23858=CARTESIAN_POINT('Ctrl Pts',(4.47711895187018,-0.503474193090318,
4.31548296397124));
#23859=CARTESIAN_POINT('Ctrl Pts',(4.46916631252638,-0.450946196152703,
4.39931155029312));
#23860=CARTESIAN_POINT('Ctrl Pts',(4.46121367318257,-0.377027575114933,
4.46973651511953));
#23861=CARTESIAN_POINT('Ctrl Pts',(4.45326103383876,-0.290755888038263,
4.51814744739689));
#23862=CARTESIAN_POINT('Ctrl Pts',(4.44530839449495,-0.204484200961595,
4.56655837967425));
#23863=CARTESIAN_POINT('Ctrl Pts',(4.43735575515115,-0.105859447846027,
4.59295527940255));
#23864=CARTESIAN_POINT('Ctrl Pts',(4.42940311580734,-0.00693984821361558,
4.59411076594835));
#23865=CARTESIAN_POINT('Ctrl Pts',(4.42921721429075,-0.0046274959494805,
4.59413777669183));
#23866=CARTESIAN_POINT('Ctrl Pts',(4.42903131277416,-0.00231498256911503,
4.59415099449182));
#23867=CARTESIAN_POINT('Ctrl Pts',(4.42884541125756,-2.46302091461148E-6,
4.59415045696459));
#23868=CARTESIAN_POINT('Ctrl Pts',(4.32115458874249,3.58587963140688E-6,
4.59404994535016));
#23869=CARTESIAN_POINT('Ctrl Pts',(4.32544000997495,-0.0533308355660028,
4.59403876103764));
#23870=CARTESIAN_POINT('Ctrl Pts',(4.3297254312074,-0.106668183692779,4.58692369872924));
#23871=CARTESIAN_POINT('Ctrl Pts',(4.33401085243985,-0.158055593105036,
4.57274269264177));
#23872=CARTESIAN_POINT('Ctrl Pts',(4.34196349178366,-0.253417405095285,
4.54642639353635));
#23873=CARTESIAN_POINT('Ctrl Pts',(4.34991613112746,-0.342064054954561,
4.49577653064689));
#23874=CARTESIAN_POINT('Ctrl Pts',(4.35786877047127,-0.413157291282808,
4.42698573291487));
#23875=CARTESIAN_POINT('Ctrl Pts',(4.36582140981507,-0.484250527611055,
4.35819493518285));
#23876=CARTESIAN_POINT('Ctrl Pts',(4.37377404915888,-0.537790350408272,
4.27126320260829));
#23877=CARTESIAN_POINT('Ctrl Pts',(4.38172668850269,-0.567230782432438,
4.17681912699824));
#23878=CARTESIAN_POINT('Ctrl Pts',(4.3896793278465,-0.596671214456604,4.0823750513882));
#23879=CARTESIAN_POINT('Ctrl Pts',(4.3976319671903,-0.602012255707717,3.98041863274268));
#23880=CARTESIAN_POINT('Ctrl Pts',(4.40558460653411,-0.582600893642323,
3.88341542999892));
#23881=CARTESIAN_POINT('Ctrl Pts',(4.41353724587791,-0.563189531576929,
3.78641222725516));
#23882=CARTESIAN_POINT('Ctrl Pts',(4.42148988522172,-0.519025766195027,
3.69436224041317));
#23883=CARTESIAN_POINT('Ctrl Pts',(4.42944252456553,-0.455509217992651,
3.61851983504546));
#23884=CARTESIAN_POINT('Ctrl Pts',(4.43739516390933,-0.391992669790276,
3.54267742967776));
#23885=CARTESIAN_POINT('Ctrl Pts',(4.44534780325314,-0.309123338767427,
3.48304260578434));
#23886=CARTESIAN_POINT('Ctrl Pts',(4.45330044259694,-0.217033129998519,
3.44690653227429));
#23887=CARTESIAN_POINT('Ctrl Pts',(4.46125308194075,-0.12494292122961,3.41077045876423));
#23888=CARTESIAN_POINT('Ctrl Pts',(4.46920572128456,-0.0236318347146405,
3.39813313563753));
#23889=CARTESIAN_POINT('Ctrl Pts',(4.47715836062837,0.074513469760962,3.41053964803971));
#23890=CARTESIAN_POINT('Ctrl Pts',(4.48511099997217,0.172658774236564,3.42294616044189));
#23891=CARTESIAN_POINT('Ctrl Pts',(4.49306363931598,0.2676382966728,3.46039650837296));
#23892=CARTESIAN_POINT('Ctrl Pts',(4.50101627865978,0.34783949666059,3.51831187658845));
#23893=CARTESIAN_POINT('Ctrl Pts',(4.50896891800359,0.428040696648381,3.57622724480394));
#23894=CARTESIAN_POINT('Ctrl Pts',(4.51692155734739,0.493463574187728,3.65460763330386));
#23895=CARTESIAN_POINT('Ctrl Pts',(4.5248741966912,0.536109291561612,3.74386997215216));
#23896=CARTESIAN_POINT('Ctrl Pts',(4.53282683603501,0.578755008935497,3.83313231100046));
#23897=CARTESIAN_POINT('Ctrl Pts',(4.54077947537881,0.598623566143919,3.93327660019715));
#23898=CARTESIAN_POINT('Ctrl Pts',(4.54873211472262,0.593285761408823,4.03205883640902));
#23899=CARTESIAN_POINT('Ctrl Pts',(4.55668475406643,0.587947956673727,4.1308410726209));
#23900=CARTESIAN_POINT('Ctrl Pts',(4.56463739341024,0.557403789995114,4.22826125584796));
#23901=CARTESIAN_POINT('Ctrl Pts',(4.57259003275404,0.505387701781775,4.31240844187621));
#23902=CARTESIAN_POINT('Ctrl Pts',(4.58054267209785,0.453371613568435,4.39655562790445));
#23903=CARTESIAN_POINT('Ctrl Pts',(4.58849531144165,0.37988360382037,4.46742981673387));
#23904=CARTESIAN_POINT('Ctrl Pts',(4.59644795078546,0.293908582600447,4.51636567348148));
#23905=CARTESIAN_POINT('Ctrl Pts',(4.60440059012926,0.207933561380525,4.56530153022909));
#23906=CARTESIAN_POINT('Ctrl Pts',(4.61235322947307,0.109471528688745,4.59229905489488));
#23907=CARTESIAN_POINT('Ctrl Pts',(4.62030586881688,0.01056080905581,4.59405743239568));
#23908=CARTESIAN_POINT('Ctrl Pts',(4.62058877545875,0.00704216595801619,
4.59411998479525));
#23909=CARTESIAN_POINT('Ctrl Pts',(4.62087168210062,0.00352295504485493,
4.59415059693914));
#23910=CARTESIAN_POINT('Ctrl Pts',(4.62115458874249,3.7232086238465E-6,
4.59414939806979));
#23911=CARTESIAN_POINT('Origin',(4.,0.,4.));
#23912=CARTESIAN_POINT('',(5.02884541125756,1.1583539301252E-5,4.59413174414479));
#23913=CARTESIAN_POINT('',(4.92115458874249,-9.52916733652962E-6,4.59405847898621));
#23914=CARTESIAN_POINT('',(4.,-7.27562663373442E-17,4.5941));
#23915=CARTESIAN_POINT('Ctrl Pts',(5.02884541125756,1.1583539301252E-5,
4.59413174414479));
#23916=CARTESIAN_POINT('Ctrl Pts',(5.02784729636931,0.0124287555737821,
4.59414271605904));
#23917=CARTESIAN_POINT('Ctrl Pts',(5.02684918148107,0.024845254523583,4.59376142828251));
#23918=CARTESIAN_POINT('Ctrl Pts',(5.02585106659282,0.0372368329321061,
4.59298328977014));
#23919=CARTESIAN_POINT('Ctrl Pts',(5.01789842724901,0.135968707532707,4.58678334723719));
#23920=CARTESIAN_POINT('Ctrl Pts',(5.00994578790521,0.233118536601742,4.55538989360237));
#23921=CARTESIAN_POINT('Ctrl Pts',(5.0019931485614,0.316808430381418,4.50264120614281));
#23922=CARTESIAN_POINT('Ctrl Pts',(4.9940405092176,0.400498324161095,4.44989251868324));
#23923=CARTESIAN_POINT('Ctrl Pts',(4.98608786987379,0.470728282651411,4.37578859739892));
#23924=CARTESIAN_POINT('Ctrl Pts',(4.97813523052998,0.518911736914097,4.289389655942));
#23925=CARTESIAN_POINT('Ctrl Pts',(4.97018259118617,0.567095191176782,4.20299071448508));
#23926=CARTESIAN_POINT('Ctrl Pts',(4.96222995184237,0.593232141211837,4.10429675285556));
#23927=CARTESIAN_POINT('Ctrl Pts',(4.95427731249856,0.594126988899363,4.00537445204741));
#23928=CARTESIAN_POINT('Ctrl Pts',(4.94632467315476,0.595021836586889,3.90645215123927));
#23929=CARTESIAN_POINT('Ctrl Pts',(4.93837203381095,0.570674581926886,3.80730151125251));
#23930=CARTESIAN_POINT('Ctrl Pts',(4.93041939446714,0.524062008404491,3.72004504823011));
#23931=CARTESIAN_POINT('Ctrl Pts',(4.92246675512334,0.477449434882097,3.6327885852077));
#23932=CARTESIAN_POINT('Ctrl Pts',(4.91451411577953,0.408571542497308,3.55742629914966));
#23933=CARTESIAN_POINT('Ctrl Pts',(4.90656147643572,0.325849591692228,3.50317225594031));
#23934=CARTESIAN_POINT('Ctrl Pts',(4.89860883709192,0.243127640887147,3.44891821273095));
#23935=CARTESIAN_POINT('Ctrl Pts',(4.89065619774811,0.146561631661773,3.41577241237029));
#23936=CARTESIAN_POINT('Ctrl Pts',(4.88270355840431,0.0479580738465473,
3.40778738038914));
#23937=CARTESIAN_POINT('Ctrl Pts',(4.8747509190605,-0.0506454839686783,
3.39980234840799));
#23938=CARTESIAN_POINT('Ctrl Pts',(4.86679827971669,-0.151286590373755,
3.41697808480634));
#23939=CARTESIAN_POINT('Ctrl Pts',(4.85884564037289,-0.241660499406316,
3.45721462188069));
#23940=CARTESIAN_POINT('Ctrl Pts',(4.85089300102908,-0.332034408438876,
3.49745115895503));
#23941=CARTESIAN_POINT('Ctrl Pts',(4.84294036168527,-0.41214112009892,3.56074849670536));
#23942=CARTESIAN_POINT('Ctrl Pts',(4.83498772234147,-0.472186497854497,
3.63936767349926));
#23943=CARTESIAN_POINT('Ctrl Pts',(4.82703508299766,-0.532231875610076,
3.71798685029316));
#23944=CARTESIAN_POINT('Ctrl Pts',(4.81908244365386,-0.572215919461187,
3.81192786613063));
#23945=CARTESIAN_POINT('Ctrl Pts',(4.81112980431005,-0.587250035475296,
3.9097051523746));
#23946=CARTESIAN_POINT('Ctrl Pts',(4.80317716496624,-0.602284151489406,
4.00748243861856));
#23947=CARTESIAN_POINT('Ctrl Pts',(4.79522452562244,-0.592368339666514,
4.10909599526903));
#23948=CARTESIAN_POINT('Ctrl Pts',(4.78727188627863,-0.558714943052599,
4.20212218107662));
#23949=CARTESIAN_POINT('Ctrl Pts',(4.77931924693482,-0.525061546438685,
4.2951483668842));
#23950=CARTESIAN_POINT('Ctrl Pts',(4.77136660759101,-0.467670565033749,
4.37958718184891));
#23951=CARTESIAN_POINT('Ctrl Pts',(4.76341396824721,-0.393558827964045,
4.44511483080773));
#23952=CARTESIAN_POINT('Ctrl Pts',(4.7554613289034,-0.319447090894342,4.51064247976655));
#23953=CARTESIAN_POINT('Ctrl Pts',(4.7475086895596,-0.228614598159871,4.55725896271948));
#23954=CARTESIAN_POINT('Ctrl Pts',(4.73955605021579,-0.13216685911108,4.5792647797218));
#23955=CARTESIAN_POINT('Ctrl Pts',(4.73598583722972,-0.0888681559330128,
4.58914394690572));
#23956=CARTESIAN_POINT('Ctrl Pts',(4.73241562424364,-0.0444377444908,4.59406302997518));
#23957=CARTESIAN_POINT('Ctrl Pts',(4.72884541125756,-4.67700812217808E-6,
4.59405084457266));
#23958=CARTESIAN_POINT('Ctrl Pts',(4.62115458874249,3.7232086238465E-6,
4.59414939806979));
#23959=CARTESIAN_POINT('Ctrl Pts',(4.62882432144443,-0.0954043143036648,
4.59411689615543));
#23960=CARTESIAN_POINT('Ctrl Pts',(4.63649405414636,-0.190827729806029,
4.57070400848325));
#23961=CARTESIAN_POINT('Ctrl Pts',(4.6441637868483,-0.275369369969159,4.52648596729292));
#23962=CARTESIAN_POINT('Ctrl Pts',(4.65211642619211,-0.363029422787103,
4.48063689435358));
#23963=CARTESIAN_POINT('Ctrl Pts',(4.66006906553591,-0.438990121848901,
4.4124195181391));
#23964=CARTESIAN_POINT('Ctrl Pts',(4.66802170487971,-0.493964237128006,
4.33017434199545));
#23965=CARTESIAN_POINT('Ctrl Pts',(4.67597434422352,-0.548938352407109,
4.24792916585179));
#23966=CARTESIAN_POINT('Ctrl Pts',(4.68392698356733,-0.582925883903521,
4.15165618977896));
#23967=CARTESIAN_POINT('Ctrl Pts',(4.69187962291114,-0.591771392992132,
4.05312609631255));
#23968=CARTESIAN_POINT('Ctrl Pts',(4.69983226225494,-0.600616902080743,
3.95459600284613));
#23969=CARTESIAN_POINT('Ctrl Pts',(4.70778490159875,-0.584320388761555,
3.85380879198612));
#23970=CARTESIAN_POINT('Ctrl Pts',(4.71573754094256,-0.544874323741249,
3.76308707295491));
#23971=CARTESIAN_POINT('Ctrl Pts',(4.72369018028636,-0.505428258720944,
3.6723653539237));
#23972=CARTESIAN_POINT('Ctrl Pts',(4.73164281963017,-0.442832641999522,
3.59170912672127));
#23973=CARTESIAN_POINT('Ctrl Pts',(4.73959545897397,-0.364740640256699,
3.53097971363863));
#23974=CARTESIAN_POINT('Ctrl Pts',(4.74754809831778,-0.286648638513876,
3.47025030055599));
#23975=CARTESIAN_POINT('Ctrl Pts',(4.75550073766158,-0.193060251749651,
3.42944770159313));
#23976=CARTESIAN_POINT('Ctrl Pts',(4.76345337700539,-0.095417934894009,
3.41356059019365));
#23977=CARTESIAN_POINT('Ctrl Pts',(4.7714060163492,0.00222438196163176,
3.39767347879416));
#23978=CARTESIAN_POINT('Ctrl Pts',(4.77935865569301,0.10392062890869,3.40670185495805));
#23979=CARTESIAN_POINT('Ctrl Pts',(4.78731129503681,0.19723705468272,3.43954187673519));
#23980=CARTESIAN_POINT('Ctrl Pts',(4.79526393438062,0.290553480456751,3.47238189851233));
#23981=CARTESIAN_POINT('Ctrl Pts',(4.80321657372443,0.375490085057754,3.52903356590271));
#23982=CARTESIAN_POINT('Ctrl Pts',(4.81116921306823,0.441662211759978,3.60257044098769));
#23983=CARTESIAN_POINT('Ctrl Pts',(4.81912185241204,0.507834338462201,3.67610731607267));
#23984=CARTESIAN_POINT('Ctrl Pts',(4.82707449175584,0.555241987265645,3.76652939885225));
#23985=CARTESIAN_POINT('Ctrl Pts',(4.83502713109965,0.57808892742485,3.86278135818256));
#23986=CARTESIAN_POINT('Ctrl Pts',(4.84297977044346,0.600935867584054,3.95903331751286));
#23987=CARTESIAN_POINT('Ctrl Pts',(4.85093240978726,0.599222099099018,4.0611151533939));
#23988=CARTESIAN_POINT('Ctrl Pts',(4.85888504913107,0.573157153508111,4.15654597106253));
#23989=CARTESIAN_POINT('Ctrl Pts',(4.86683768847488,0.547092207917203,4.25197678873116));
#23990=CARTESIAN_POINT('Ctrl Pts',(4.87479032781868,0.496676085220424,4.34075658818739));
#23991=CARTESIAN_POINT('Ctrl Pts',(4.88274296716249,0.428072843071251,4.41203082979109));
#23992=CARTESIAN_POINT('Ctrl Pts',(4.89069560650629,0.359469600922078,4.48330507139479));
#23993=CARTESIAN_POINT('Ctrl Pts',(4.8986482458501,0.272679239320511,4.53707375514596));
#23994=CARTESIAN_POINT('Ctrl Pts',(4.90660088519391,0.178313062033339,4.56676292714126));
#23995=CARTESIAN_POINT('Ctrl Pts',(4.9114521197101,0.120748216373203,4.58487378690922));
#23996=CARTESIAN_POINT('Ctrl Pts',(4.9163033542263,0.0603642649825261,4.59402420038378));
#23997=CARTESIAN_POINT('Ctrl Pts',(4.92115458874249,-9.52916733652962E-6,
4.59405847898621));
#23998=CARTESIAN_POINT('Origin',(4.,0.,4.));
#23999=CARTESIAN_POINT('',(5.32884541125756,-1.45357002139801E-5,4.59407911932661));
#24000=CARTESIAN_POINT('',(5.22115458874249,1.46139895546772E-5,4.59411444380891));
#24001=CARTESIAN_POINT('',(4.,-7.27562663373442E-17,4.5941));
#24002=CARTESIAN_POINT('Ctrl Pts',(5.32884541125756,-1.45357002139801E-5,
4.59407911932661));
#24003=CARTESIAN_POINT('Ctrl Pts',(5.32327896849499,0.0692531541268509,
4.59401614001471));
#24004=CARTESIAN_POINT('Ctrl Pts',(5.31771252573242,0.138542285837495,4.5819075943171));
#24005=CARTESIAN_POINT('Ctrl Pts',(5.31214608296985,0.203593590158122,4.55818044906639));
#24006=CARTESIAN_POINT('Ctrl Pts',(5.30419344362604,0.296530782575621,4.5242820624512));
#24007=CARTESIAN_POINT('Ctrl Pts',(5.29624080428224,0.380818089806801,4.46666879957728));
#24008=CARTESIAN_POINT('Ctrl Pts',(5.28828816493843,0.446150240572578,4.39238466650784));
#24009=CARTESIAN_POINT('Ctrl Pts',(5.28033552559462,0.511482391338355,4.3181005334384));
#24010=CARTESIAN_POINT('Ctrl Pts',(5.27238288625081,0.557859385638729,4.22714553017344));
#24011=CARTESIAN_POINT('Ctrl Pts',(5.26443024690701,0.579611004278495,4.13064014464439));
#24012=CARTESIAN_POINT('Ctrl Pts',(5.2564776075632,0.601362622918262,4.03413475911534));
#24013=CARTESIAN_POINT('Ctrl Pts',(5.2485249682194,0.598488865897423,3.93207899132219));
#24014=CARTESIAN_POINT('Ctrl Pts',(5.24057232887559,0.571341089151559,3.8369505488493));
#24015=CARTESIAN_POINT('Ctrl Pts',(5.23261968953179,0.544193312405696,3.74182210637642));
#24016=CARTESIAN_POINT('Ctrl Pts',(5.22466705018798,0.492771515934809,3.65362098922379));
#24017=CARTESIAN_POINT('Ctrl Pts',(5.21671441084417,0.423362714708271,3.58313098523844));
#24018=CARTESIAN_POINT('Ctrl Pts',(5.20876177150037,0.353953913481732,3.51264098125308));
#24019=CARTESIAN_POINT('Ctrl Pts',(5.20080913215656,0.266558107499543,3.45986209043499));
#24020=CARTESIAN_POINT('Ctrl Pts',(5.19285649281275,0.171860624350003,3.43124725102074));
#24021=CARTESIAN_POINT('Ctrl Pts',(5.18490385346895,0.0771631412004631,
3.40263241160649));
#24022=CARTESIAN_POINT('Ctrl Pts',(5.17695121412514,-0.0248360191164267,
3.39818162359609));
#24023=CARTESIAN_POINT('Ctrl Pts',(5.16899857478133,-0.121666070051256,
3.41843905644231));
#24024=CARTESIAN_POINT('Ctrl Pts',(5.16104593543753,-0.218496120986084,
3.43869648928852));
#24025=CARTESIAN_POINT('Ctrl Pts',(5.15309329609372,-0.310157062538852,
3.48366214299137));
#24026=CARTESIAN_POINT('Ctrl Pts',(5.14514065674991,-0.385442096207774,
3.54783835396576));
#24027=CARTESIAN_POINT('Ctrl Pts',(5.13718801740611,-0.460727129876697,
3.61201456494015));
#24028=CARTESIAN_POINT('Ctrl Pts',(5.1292353780623,-0.519636255661773,3.6954013331861));
#24029=CARTESIAN_POINT('Ctrl Pts',(5.1212827387185,-0.554967030609594,3.78780349058054));
#24030=CARTESIAN_POINT('Ctrl Pts',(5.11333009937469,-0.590297805557415,
3.88020564797498));
#24031=CARTESIAN_POINT('Ctrl Pts',(5.10537746003088,-0.60205022966798,3.98162319451792));
#24032=CARTESIAN_POINT('Ctrl Pts',(5.09742482068708,-0.588787409028971,
4.07965645386523));
#24033=CARTESIAN_POINT('Ctrl Pts',(5.08947218134327,-0.575524588389962,
4.17768971321255));
#24034=CARTESIAN_POINT('Ctrl Pts',(5.08151954199946,-0.537246523001379,
4.27233868536424));
#24035=CARTESIAN_POINT('Ctrl Pts',(5.07356690265566,-0.47863322769376,4.35203124438164));
#24036=CARTESIAN_POINT('Ctrl Pts',(5.06561426331185,-0.42001993238614,4.43172380339905));
#24037=CARTESIAN_POINT('Ctrl Pts',(5.05766162396805,-0.341071407159484,
4.49645994928216));
#24038=CARTESIAN_POINT('Ctrl Pts',(5.04970898462424,-0.251440184480074,
4.53832480650817));
#24039=CARTESIAN_POINT('Ctrl Pts',(5.04275446016868,-0.1730583412759,4.5749353153996));
#24040=CARTESIAN_POINT('Ctrl Pts',(5.03579993571312,-0.0865070403179845,
4.59405529558476));
#24041=CARTESIAN_POINT('Ctrl Pts',(5.02884541125756,1.1583539301252E-5,
4.59413174414479));
#24042=CARTESIAN_POINT('Ctrl Pts',(4.92115458874249,-9.52916733652962E-6,
4.59405847898621));
#24043=CARTESIAN_POINT('Ctrl Pts',(4.9242559935701,-0.0386066277022544,
4.59408039337166));
#24044=CARTESIAN_POINT('Ctrl Pts',(4.92735739839772,-0.0771995748988638,
4.59037647703175));
#24045=CARTESIAN_POINT('Ctrl Pts',(4.93045880322533,-0.115049119822012,
4.58290605049323));
#24046=CARTESIAN_POINT('Ctrl Pts',(4.93841144256913,-0.212103131417409,
4.56375034161047));
#24047=CARTESIAN_POINT('Ctrl Pts',(4.94636408191294,-0.304269161635426,
4.51982926360553));
#24048=CARTESIAN_POINT('Ctrl Pts',(4.95431672125675,-0.380278658005779,
4.45651276645759));
#24049=CARTESIAN_POINT('Ctrl Pts',(4.96226936060055,-0.456288154376132,
4.39319626930964));
#24050=CARTESIAN_POINT('Ctrl Pts',(4.97022199994436,-0.516141116898821,
4.31048435301868));
#24051=CARTESIAN_POINT('Ctrl Pts',(4.97817463928816,-0.552519705724467,
4.21848967586497));
#24052=CARTESIAN_POINT('Ctrl Pts',(4.98612727863197,-0.588898294550112,
4.12649499871126));
#24053=CARTESIAN_POINT('Ctrl Pts',(4.99407991797578,-0.601802509678713,
4.0252175606948));
#24054=CARTESIAN_POINT('Ctrl Pts',(5.00203255731958,-0.589654635058918,
3.92703990798411));
#24055=CARTESIAN_POINT('Ctrl Pts',(5.00998519666339,-0.577506760439122,
3.82886225527341));
#24056=CARTESIAN_POINT('Ctrl Pts',(5.0179378360072,-0.540306796070929,3.73378438786847));
#24057=CARTESIAN_POINT('Ctrl Pts',(5.025890475351,-0.482602944251693,3.65343086999412));
#24058=CARTESIAN_POINT('Ctrl Pts',(5.03384311469481,-0.424899092432456,
3.57307735211977));
#24059=CARTESIAN_POINT('Ctrl Pts',(5.04179575403862,-0.346691353162178,
3.50744818377599));
#24060=CARTESIAN_POINT('Ctrl Pts',(5.04974839338242,-0.257541687734669,
3.46456742464414));
#24061=CARTESIAN_POINT('Ctrl Pts',(5.05770103272623,-0.16839202230716,3.42168666551229));
#24062=CARTESIAN_POINT('Ctrl Pts',(5.06565367207003,-0.0683004307224215,
3.40155431559236));
#24063=CARTESIAN_POINT('Ctrl Pts',(5.07360631141384,0.0304955267282049,
3.40663182885918));
#24064=CARTESIAN_POINT('Ctrl Pts',(5.08155895075765,0.129291484178831,3.41170934212599));
#24065=CARTESIAN_POINT('Ctrl Pts',(5.08951159010146,0.226791807495345,3.44199671857955));
#24066=CARTESIAN_POINT('Ctrl Pts',(5.09746422944526,0.311075754224562,3.49379091394262));
#24067=CARTESIAN_POINT('Ctrl Pts',(5.10541686878907,0.395359700953779,3.54558510930568));
#24068=CARTESIAN_POINT('Ctrl Pts',(5.11336950813287,0.466427271095698,3.61888612357825));
#24069=CARTESIAN_POINT('Ctrl Pts',(5.12132214747668,0.515589486279599,3.70473190942573));
#24070=CARTESIAN_POINT('Ctrl Pts',(5.12927478682048,0.564751701463499,3.79057769527322));
#24071=CARTESIAN_POINT('Ctrl Pts',(5.13722742616429,0.592008561689381,3.88896825269562));
#24072=CARTESIAN_POINT('Ctrl Pts',(5.1451800655081,0.594027544563649,3.98787399599556));
#24073=CARTESIAN_POINT('Ctrl Pts',(5.1531327048519,0.596046527437917,4.0867797392955));
#24074=CARTESIAN_POINT('Ctrl Pts',(5.16108534419571,0.572827632960568,4.18620066847299));
#24075=CARTESIAN_POINT('Ctrl Pts',(5.16903798353952,0.527209687216453,4.2739812208502));
#24076=CARTESIAN_POINT('Ctrl Pts',(5.17699062288332,0.481591741472338,4.3617617732274));
#24077=CARTESIAN_POINT('Ctrl Pts',(5.18494326222713,0.413574744461461,4.43790194880433));
#24078=CARTESIAN_POINT('Ctrl Pts',(5.19289590157094,0.331474700441294,4.49309257410834));
#24079=CARTESIAN_POINT('Ctrl Pts',(5.20084854091474,0.24937465642113,4.54828319941234));
#24080=CARTESIAN_POINT('Ctrl Pts',(5.20880118025855,0.153191565391677,4.58252427444343));
#24081=CARTESIAN_POINT('Ctrl Pts',(5.21675381960235,0.0546851202186884,
4.59162936142496));
#24082=CARTESIAN_POINT('Ctrl Pts',(5.21822074264906,0.0365148790664279,
4.59330886194775));
#24083=CARTESIAN_POINT('Ctrl Pts',(5.21968766569578,0.018265586889787,4.59413312238171));
#24084=CARTESIAN_POINT('Ctrl Pts',(5.22115458874249,1.46139895546772E-5,
4.59411444380891));
#24085=CARTESIAN_POINT('Origin',(4.,0.,4.));
#24086=CARTESIAN_POINT('',(5.62884541125756,1.52328526200479E-5,4.59408648697874));
#24087=CARTESIAN_POINT('',(5.52115458874249,-1.55733839743342E-5,4.59409663347568));
#24088=CARTESIAN_POINT('',(4.,-7.27562663373442E-17,4.5941));
#24089=CARTESIAN_POINT('Ctrl Pts',(5.62884541125756,1.52328526200479E-5,
4.59408648697874));
#24090=CARTESIAN_POINT('Ctrl Pts',(5.62666327996447,0.0271682673899915,
4.59411287463303));
#24091=CARTESIAN_POINT('Ctrl Pts',(5.62448114867138,0.054317778225707,4.59228554395034));
#24092=CARTESIAN_POINT('Ctrl Pts',(5.62229901737829,0.0812075234320336,
4.58857548522516));
#24093=CARTESIAN_POINT('Ctrl Pts',(5.61434637803449,0.179205497408217,4.57505441109036));
#24094=CARTESIAN_POINT('Ctrl Pts',(5.60639373869068,0.273753285393806,4.53652709601604));
#24095=CARTESIAN_POINT('Ctrl Pts',(5.59844109934688,0.353291132582354,4.47770402899113));
#24096=CARTESIAN_POINT('Ctrl Pts',(5.59048846000307,0.432828979770902,4.41888096196622));
#24097=CARTESIAN_POINT('Ctrl Pts',(5.58253582065927,0.497356886162411,4.33976214299073));
#24098=CARTESIAN_POINT('Ctrl Pts',(5.57458318131546,0.538985436353474,4.25002092526659));
#24099=CARTESIAN_POINT('Ctrl Pts',(5.56663054197165,0.580613986544537,4.16027970754245));
#24100=CARTESIAN_POINT('Ctrl Pts',(5.55867790262784,0.599343180535155,4.05991609106967));
#24101=CARTESIAN_POINT('Ctrl Pts',(5.55072526328404,0.592883119270616,3.96120089488413));
#24102=CARTESIAN_POINT('Ctrl Pts',(5.54277262394023,0.586423058006077,3.86248569869858));
#24103=CARTESIAN_POINT('Ctrl Pts',(5.53481998459642,0.554773741486382,3.76541892280029));
#24104=CARTESIAN_POINT('Ctrl Pts',(5.52686734525262,0.501804729712613,3.68186830256729));
#24105=CARTESIAN_POINT('Ctrl Pts',(5.51891470590881,0.448835717938844,3.5983176823343));
#24106=CARTESIAN_POINT('Ctrl Pts',(5.51096206656501,0.374547010911001,3.52828321776661));
#24107=CARTESIAN_POINT('Ctrl Pts',(5.5030094272212,0.288021414854312,3.48032757600706));
#24108=CARTESIAN_POINT('Ctrl Pts',(5.4950567878774,0.201495818797622,3.4323719342475));
#24109=CARTESIAN_POINT('Ctrl Pts',(5.48710414853359,0.102733333712086,3.40649511529609));
#24110=CARTESIAN_POINT('Ctrl Pts',(5.47915150918978,0.00380901851787326,
3.40586091270526));
#24111=CARTESIAN_POINT('Ctrl Pts',(5.47119886984597,-0.0951152966763399,
3.40522671011442));
#24112=CARTESIAN_POINT('Ctrl Pts',(5.46324623050217,-0.194201441979227,
3.42983512388417));
#24113=CARTESIAN_POINT('Ctrl Pts',(5.45529359115836,-0.281334786601535,
3.47667744027106));
#24114=CARTESIAN_POINT('Ctrl Pts',(5.44734095181456,-0.368468131223842,
3.52351975665794));
#24115=CARTESIAN_POINT('Ctrl Pts',(5.43938831247075,-0.443648675165568,
3.59259597566196));
#24116=CARTESIAN_POINT('Ctrl Pts',(5.43143567312694,-0.497684572991269,
3.67546058871077));
#24117=CARTESIAN_POINT('Ctrl Pts',(5.42348303378314,-0.551720470816969,
3.75832520175959));
#24118=CARTESIAN_POINT('Ctrl Pts',(5.41553039443933,-0.584611722526643,
3.85497820885321));
#24119=CARTESIAN_POINT('Ctrl Pts',(5.40757775509553,-0.592336924628993,
3.95360246348684));
#24120=CARTESIAN_POINT('Ctrl Pts',(5.39962511575172,-0.600062126731343,
4.05222671812048));
#24121=CARTESIAN_POINT('Ctrl Pts',(5.39167247640791,-0.582621279226368,
4.15282222029412));
#24122=CARTESIAN_POINT('Ctrl Pts',(5.3837198370641,-0.542146763261091,4.24308979978386));
#24123=CARTESIAN_POINT('Ctrl Pts',(5.3757671977203,-0.501672247295815,4.3333573792736));
#24124=CARTESIAN_POINT('Ctrl Pts',(5.36781455837649,-0.438164062870237,
4.41329703607943));
#24125=CARTESIAN_POINT('Ctrl Pts',(5.35986191903269,-0.359386950494509,
4.47313505840055));
#24126=CARTESIAN_POINT('Ctrl Pts',(5.35190927968888,-0.28060983811878,4.53297308072167));
#24127=CARTESIAN_POINT('Ctrl Pts',(5.34395664034507,-0.1865637977929,4.57270946855809));
#24128=CARTESIAN_POINT('Ctrl Pts',(5.33600400100126,-0.0887472388280498,
4.58748590729807));
#24129=CARTESIAN_POINT('Ctrl Pts',(5.33361780442003,-0.0593972924141157,
4.59191959101989));
#24130=CARTESIAN_POINT('Ctrl Pts',(5.3312316078388,-0.0297078841644672,
4.59410611700271));
#24131=CARTESIAN_POINT('Ctrl Pts',(5.32884541125756,-1.45357002139801E-5,
4.59407911932661));
#24132=CARTESIAN_POINT('Ctrl Pts',(5.22115458874249,1.46139895546772E-5,
4.59411444380891));
#24133=CARTESIAN_POINT('Ctrl Pts',(5.22764030503958,-0.0806785298274998,
4.59403186011492));
#24134=CARTESIAN_POINT('Ctrl Pts',(5.23412602133668,-0.161404528346198,
4.57747154641029));
#24135=CARTESIAN_POINT('Ctrl Pts',(5.24061173763377,-0.235476461490165,
4.54549665421293));
#24136=CARTESIAN_POINT('Ctrl Pts',(5.24856437697758,-0.32630179870949,4.50628976108741));
#24137=CARTESIAN_POINT('Ctrl Pts',(5.25651701632139,-0.407122673831612,
4.44390687590439));
#24138=CARTESIAN_POINT('Ctrl Pts',(5.26446965566519,-0.468057634114636,
4.36597515601533));
#24139=CARTESIAN_POINT('Ctrl Pts',(5.272422295009,-0.52899259439766,4.28804343612627));
#24140=CARTESIAN_POINT('Ctrl Pts',(5.28037493435281,-0.570041639841584,
4.19456288153117));
#24141=CARTESIAN_POINT('Ctrl Pts',(5.28832757369661,-0.586185965564114,
4.09696276320888));
#24142=CARTESIAN_POINT('Ctrl Pts',(5.29628021304042,-0.602330291286644,
3.99936264488659));
#24143=CARTESIAN_POINT('Ctrl Pts',(5.30423285238423,-0.59356989728778,3.89764296283709));
#24144=CARTESIAN_POINT('Ctrl Pts',(5.31218549172803,-0.560975861048054,
3.80424033358521));
#24145=CARTESIAN_POINT('Ctrl Pts',(5.32013813107184,-0.528381824808328,
3.71083770433334));
#24146=CARTESIAN_POINT('Ctrl Pts',(5.32809077041564,-0.471954146327742,
3.62575212787907));
#24147=CARTESIAN_POINT('Ctrl Pts',(5.33604340975945,-0.398591877830097,
3.55938647478623));
#24148=CARTESIAN_POINT('Ctrl Pts',(5.34399604910326,-0.325229609332449,
3.49302082169338));
#24149=CARTESIAN_POINT('Ctrl Pts',(5.35194868844707,-0.234932750817741,
3.44537509196196));
#24150=CARTESIAN_POINT('Ctrl Pts',(5.35990132779087,-0.138741323057917,
3.42227462497344));
#24151=CARTESIAN_POINT('Ctrl Pts',(5.36785396713468,-0.042549895298095,
3.39917415798493));
#24152=CARTESIAN_POINT('Ctrl Pts',(5.37580660647848,0.059536101706843,3.40061895373932));
#24153=CARTESIAN_POINT('Ctrl Pts',(5.38375924582229,0.155035264439678,3.42643236627792));
#24154=CARTESIAN_POINT('Ctrl Pts',(5.39171188516609,0.250534427172515,3.45224577881651));
#24155=CARTESIAN_POINT('Ctrl Pts',(5.3996645245099,0.339446755633248,3.5024278081393));
#24156=CARTESIAN_POINT('Ctrl Pts',(5.40761716385371,0.41090150670596,3.57084301769608));
#24157=CARTESIAN_POINT('Ctrl Pts',(5.41556980319751,0.482356257778672,3.63925822725286));
#24158=CARTESIAN_POINT('Ctrl Pts',(5.42352244254132,0.536353431463363,3.72590661704362));
#24159=CARTESIAN_POINT('Ctrl Pts',(5.43147508188513,0.566291137850326,3.82019424128906));
#24160=CARTESIAN_POINT('Ctrl Pts',(5.43942772122893,0.596228844237288,3.91448186553449));
#24161=CARTESIAN_POINT('Ctrl Pts',(5.44738036057274,0.602107083326521,4.01640872423458));
#24162=CARTESIAN_POINT('Ctrl Pts',(5.45533299991655,0.583207160329387,4.11351287069736));
#24163=CARTESIAN_POINT('Ctrl Pts',(5.46328563926035,0.564307237332252,4.21061701716013));
#24164=CARTESIAN_POINT('Ctrl Pts',(5.47123827860416,0.520629152248751,4.30289845138559));
#24165=CARTESIAN_POINT('Ctrl Pts',(5.47919091794796,0.457513145863858,4.37907451119169));
#24166=CARTESIAN_POINT('Ctrl Pts',(5.48714355729177,0.394397139478966,4.45525057099779));
#24167=CARTESIAN_POINT('Ctrl Pts',(5.49509619663558,0.311843211792683,4.51532125638452));
#24168=CARTESIAN_POINT('Ctrl Pts',(5.50304883597938,0.219944704826683,4.5519421079172));
#24169=CARTESIAN_POINT('Ctrl Pts',(5.50908408690042,0.150203009669811,4.5797336395568));
#24170=CARTESIAN_POINT('Ctrl Pts',(5.51511933782146,0.0750795109720808,
4.59401975858331));
#24171=CARTESIAN_POINT('Ctrl Pts',(5.52115458874249,-1.55733839743342E-5,
4.59409663347568));
#24172=CARTESIAN_POINT('Origin',(4.,0.,4.));
#24173=CARTESIAN_POINT('',(5.92884541125757,-1.3134308860685E-5,4.59412454375027));
#24174=CARTESIAN_POINT('',(5.82115458874249,1.31105368646138E-5,4.59407040741879));
#24175=CARTESIAN_POINT('',(4.,-7.27562663373442E-17,4.5941));
#24176=CARTESIAN_POINT('Ctrl Pts',(5.92884541125757,-1.3134308860685E-5,
4.59412454375027));
#24177=CARTESIAN_POINT('Ctrl Pts',(5.92209495209015,0.0839697382976411,
4.5940436242297));
#24178=CARTESIAN_POINT('Ctrl Pts',(5.91534449292274,0.16798613900316,4.57606223573506));
#24179=CARTESIAN_POINT('Ctrl Pts',(5.90859403375532,0.244517407380453,4.54150437939301));
#24180=CARTESIAN_POINT('Ctrl Pts',(5.90064139441152,0.334678026211646,4.50079216098422));
#24181=CARTESIAN_POINT('Ctrl Pts',(5.89268875506771,0.41445008323119,4.43707358099086));
#24182=CARTESIAN_POINT('Ctrl Pts',(5.8847361157239,0.474080337065587,4.35813908232779));
#24183=CARTESIAN_POINT('Ctrl Pts',(5.8767834763801,0.533710590899983,4.27920458366471));
#24184=CARTESIAN_POINT('Ctrl Pts',(5.86883083703629,0.573199041549232,4.18505416633191));
#24185=CARTESIAN_POINT('Ctrl Pts',(5.86087819769249,0.587717699183782,4.08719901244189));
#24186=CARTESIAN_POINT('Ctrl Pts',(5.85292555834868,0.602236356818331,3.98934385855186));
#24187=CARTESIAN_POINT('Ctrl Pts',(5.84497291900487,0.591785221438181,3.88778396810461));
#24188=CARTESIAN_POINT('Ctrl Pts',(5.83702027966107,0.557642080814915,3.79493641494568));
#24189=CARTESIAN_POINT('Ctrl Pts',(5.82906764031726,0.523498940191649,3.70208886178675));
#24190=CARTESIAN_POINT('Ctrl Pts',(5.82111500097346,0.465663794325265,3.61795364591614));
#24191=CARTESIAN_POINT('Ctrl Pts',(5.81316236162965,0.391207780605707,3.55281744653948));
#24192=CARTESIAN_POINT('Ctrl Pts',(5.80520972228584,0.31675176688615,3.48768124716281));
#24193=CARTESIAN_POINT('Ctrl Pts',(5.79725708294203,0.225674885313418,3.44154406428009));
#24194=CARTESIAN_POINT('Ctrl Pts',(5.78930444359823,0.129112523455512,3.42004679519738));
#24195=CARTESIAN_POINT('Ctrl Pts',(5.78135180425442,0.0325501615976049,
3.39854952611466));
#24196=CARTESIAN_POINT('Ctrl Pts',(5.77339916491062,-0.0694976805454773,
3.40169217083197));
#24197=CARTESIAN_POINT('Ctrl Pts',(5.76544652556681,-0.164554263536051,
3.42909049911887));
#24198=CARTESIAN_POINT('Ctrl Pts',(5.75749388622301,-0.259610846526622,
3.45648882740576));
#24199=CARTESIAN_POINT('Ctrl Pts',(5.7495412468792,-0.347676170364685,3.50814283926225));
#24200=CARTESIAN_POINT('Ctrl Pts',(5.74158860753539,-0.417983050247216,
3.57773712775495));
#24201=CARTESIAN_POINT('Ctrl Pts',(5.73363596819158,-0.488289930129746,
3.64733141624764));
#24202=CARTESIAN_POINT('Ctrl Pts',(5.72568332884778,-0.540838366056745,
3.73486598137654));
#24203=CARTESIAN_POINT('Ctrl Pts',(5.71773068950397,-0.569203595796233,
3.82963853060694));
#24204=CARTESIAN_POINT('Ctrl Pts',(5.70977805016017,-0.597568825535722,
3.92441107983734));
#24205=CARTESIAN_POINT('Ctrl Pts',(5.70182541081636,-0.6017508490877,4.02642161316923));
#24206=CARTESIAN_POINT('Ctrl Pts',(5.69387277147255,-0.581238357244447,
4.12319795341528));
#24207=CARTESIAN_POINT('Ctrl Pts',(5.68592013212875,-0.560725865401195,
4.21997429366132));
#24208=CARTESIAN_POINT('Ctrl Pts',(5.67796749278494,-0.515518858162713,
4.31151644082153));
#24209=CARTESIAN_POINT('Ctrl Pts',(5.67001485344113,-0.451144507802385,
4.38663212069642));
#24210=CARTESIAN_POINT('Ctrl Pts',(5.66206221409732,-0.386770157442057,
4.46174780057131));
#24211=CARTESIAN_POINT('Ctrl Pts',(5.65410957475352,-0.303228463959881,
4.52043701316089));
#24212=CARTESIAN_POINT('Ctrl Pts',(5.64615693540972,-0.210733537235404,
4.55552420285805));
#24213=CARTESIAN_POINT('Ctrl Pts',(5.640386427359,-0.143618370026196,4.5809837895275));
#24214=CARTESIAN_POINT('Ctrl Pts',(5.63461591930828,-0.07178924788396,4.59401670649762));
#24215=CARTESIAN_POINT('Ctrl Pts',(5.62884541125756,1.52328526200479E-5,
4.59408648697874));
#24216=CARTESIAN_POINT('Ctrl Pts',(5.52115458874249,-1.55733839743342E-5,
4.59409663347568));
#24217=CARTESIAN_POINT('Ctrl Pts',(5.52307197716526,-0.0238731473664388,
4.59412105649149));
#24218=CARTESIAN_POINT('Ctrl Pts',(5.52498936558803,-0.0477278534282068,
4.59271130989713));
#24219=CARTESIAN_POINT('Ctrl Pts',(5.5269067540108,-0.0714062077139717,
4.58984482465595));
#24220=CARTESIAN_POINT('Ctrl Pts',(5.53485939335461,-0.169615527042917,
4.57795567218339));
#24221=CARTESIAN_POINT('Ctrl Pts',(5.54281203269841,-0.264791079455087,
4.54100634955965));
#24222=CARTESIAN_POINT('Ctrl Pts',(5.55076467204222,-0.345296357402727,
4.48351441471562));
#24223=CARTESIAN_POINT('Ctrl Pts',(5.55871731138603,-0.425801635350366,
4.4260224798716));
#24224=CARTESIAN_POINT('Ctrl Pts',(5.56666995072984,-0.491636638833473,
4.34798793280729));
#24225=CARTESIAN_POINT('Ctrl Pts',(5.57462259007364,-0.534752142022197,
4.2589515597096));
#24226=CARTESIAN_POINT('Ctrl Pts',(5.58257522941745,-0.577867645210921,
4.16991518661191));
#24227=CARTESIAN_POINT('Ctrl Pts',(5.59052786876125,-0.598263648105263,
4.06987698748084));
#24228=CARTESIAN_POINT('Ctrl Pts',(5.59848050810506,-0.59344646156208,3.97106799465478));
#24229=CARTESIAN_POINT('Ctrl Pts',(5.60643314744886,-0.588629275018896,
3.87225900182873));
#24230=CARTESIAN_POINT('Ctrl Pts',(5.61438578679267,-0.558598899038186,
3.77467921530768));
#24231=CARTESIAN_POINT('Ctrl Pts',(5.62233842613648,-0.50702695609161,3.69025909300064));
#24232=CARTESIAN_POINT('Ctrl Pts',(5.63029106548029,-0.455455013145033,
3.6058389706936));
#24233=CARTESIAN_POINT('Ctrl Pts',(5.63824370482409,-0.382341503232591,
3.53457851260056));
#24234=CARTESIAN_POINT('Ctrl Pts',(5.6461963441679,-0.296625548722353,3.48519028027742));
#24235=CARTESIAN_POINT('Ctrl Pts',(5.6541489835117,-0.210909594212113,3.43580204795428));
#24236=CARTESIAN_POINT('Ctrl Pts',(5.66210162285551,-0.112591195104077,
3.40828604140104));
#24237=CARTESIAN_POINT('Ctrl Pts',(5.67005426219932,-0.0136911147678568,
3.40600646716786));
#24238=CARTESIAN_POINT('Ctrl Pts',(5.67800690154312,0.0852089655683624,
3.40372689293467));
#24239=CARTESIAN_POINT('Ctrl Pts',(5.68595954088693,0.184690727132768,3.42668375102154));
#24240=CARTESIAN_POINT('Ctrl Pts',(5.69391218023074,0.272591169676606,3.47207025288287));
#24241=CARTESIAN_POINT('Ctrl Pts',(5.70186481957454,0.360491612220445,3.51745675474419));
#24242=CARTESIAN_POINT('Ctrl Pts',(5.70981745891835,0.436810735743714,3.58527290037998));
#24243=CARTESIAN_POINT('Ctrl Pts',(5.71777009826216,0.492217487918224,3.667227242308));
#24244=CARTESIAN_POINT('Ctrl Pts',(5.72572273760596,0.547624240092733,3.74918158423602));
#24245=CARTESIAN_POINT('Ctrl Pts',(5.73367537694977,0.582118620918482,3.84527412245626));
#24246=CARTESIAN_POINT('Ctrl Pts',(5.74162801629357,0.591483222595687,3.94375623549444));
#24247=CARTESIAN_POINT('Ctrl Pts',(5.74958065563738,0.600847824272892,4.04223834853263));
#24248=CARTESIAN_POINT('Ctrl Pts',(5.75753329498119,0.585082646801554,4.14311003638875));
#24249=CARTESIAN_POINT('Ctrl Pts',(5.76548593432499,0.546115197731279,4.23403836123177));
#24250=CARTESIAN_POINT('Ctrl Pts',(5.7734385736688,0.507147748661005,4.32496668607478));
#24251=CARTESIAN_POINT('Ctrl Pts',(5.78139121301261,0.444978027991796,4.4059516479047));
#24252=CARTESIAN_POINT('Ctrl Pts',(5.78934385235641,0.367207131024688,4.46709173242012));
#24253=CARTESIAN_POINT('Ctrl Pts',(5.79729649170022,0.28943623405758,4.52823181693554));
#24254=CARTESIAN_POINT('Ctrl Pts',(5.80524913104403,0.196064160792572,4.56952702413646));
#24255=CARTESIAN_POINT('Ctrl Pts',(5.81320177038783,0.0985069184831505,
4.58592845199323));
#24256=CARTESIAN_POINT('Ctrl Pts',(5.81585270983939,0.0659871057213339,
4.59139571767544));
#24257=CARTESIAN_POINT('Ctrl Pts',(5.81850364929094,0.0330022532417819,
4.59409688335147));
#24258=CARTESIAN_POINT('Ctrl Pts',(5.82115458874249,1.31105368646138E-5,
4.59407040741879));
#24259=CARTESIAN_POINT('Origin',(4.,0.,4.));
#24260=CARTESIAN_POINT('',(6.22884541125756,-1.27841859475647E-5,4.5940334609955));
#24261=CARTESIAN_POINT('',(6.12115458874249,-9.50793186244619E-6,4.59413936148612));
#24262=CARTESIAN_POINT('',(4.,-7.27562663373442E-17,4.5941));
#24263=CARTESIAN_POINT('Ctrl Pts',(6.22884541125756,-1.27841859475647E-5,
4.5940334609955));
#24264=CARTESIAN_POINT('Ctrl Pts',(6.22547926355963,0.0418951881409122,
4.59406590912705));
#24265=CARTESIAN_POINT('Ctrl Pts',(6.2221131158617,0.0838018877146867,4.58971510200585));
#24266=CARTESIAN_POINT('Ctrl Pts',(6.21874696816377,0.124749109322564,4.58093223526196));
#24267=CARTESIAN_POINT('Ctrl Pts',(6.21079432881996,0.22148832423537,4.56018241146135));
#24268=CARTESIAN_POINT('Ctrl Pts',(6.20284168947616,0.31287214740051,4.51469474440412));
#24269=CARTESIAN_POINT('Ctrl Pts',(6.19488905013236,0.387808805213989,4.4501133836823));
#24270=CARTESIAN_POINT('Ctrl Pts',(6.18693641078855,0.462745463027469,4.38553202296047));
#24271=CARTESIAN_POINT('Ctrl Pts',(6.17898377144474,0.521234955489287,4.30185696857405));
#24272=CARTESIAN_POINT('Ctrl Pts',(6.17103113210093,0.556083161424236,4.20927485003939));
#24273=CARTESIAN_POINT('Ctrl Pts',(6.16307849275713,0.590931367359184,4.11669273150472));
#24274=CARTESIAN_POINT('Ctrl Pts',(6.15512585341332,0.602138286767263,4.0152035488218));
#24275=CARTESIAN_POINT('Ctrl Pts',(6.14717321406952,0.588356486924291,3.9172389266648));
#24276=CARTESIAN_POINT('Ctrl Pts',(6.13922057472571,0.574574687081318,3.81927430450779));
#24277=CARTESIAN_POINT('Ctrl Pts',(6.1312679353819,0.535804167987293,3.7248342428767));
#24278=CARTESIAN_POINT('Ctrl Pts',(6.12331529603809,0.476773096629474,3.64545304401991));
#24279=CARTESIAN_POINT('Ctrl Pts',(6.11536265669429,0.417742025271657,3.56607184516312));
#24280=CARTESIAN_POINT('Ctrl Pts',(6.10741001735048,0.338450401650047,3.50174950908064));
#24281=CARTESIAN_POINT('Ctrl Pts',(6.09945737800668,0.248599092144812,3.46035682177302));
#24282=CARTESIAN_POINT('Ctrl Pts',(6.09150473866287,0.158747782639575,3.41896413446539));
#24283=CARTESIAN_POINT('Ctrl Pts',(6.08355209931906,0.0583367872507115,
3.40050109593262));
#24284=CARTESIAN_POINT('Ctrl Pts',(6.07559945997526,-0.0403606640336046,
3.40722161935946));
#24285=CARTESIAN_POINT('Ctrl Pts',(6.06764682063145,-0.139058115317921,
3.4139421427863));
#24286=CARTESIAN_POINT('Ctrl Pts',(6.05969418128764,-0.23604202249769,3.44584622817275));
#24287=CARTESIAN_POINT('Ctrl Pts',(6.05174154194384,-0.319452991027635,
3.49903499090221));
#24288=CARTESIAN_POINT('Ctrl Pts',(6.04378890260003,-0.40286395955758,3.55222375363166));
#24289=CARTESIAN_POINT('Ctrl Pts',(6.03583626325623,-0.472701989437702,
3.62669719370411));
#24290=CARTESIAN_POINT('Ctrl Pts',(6.02788362391242,-0.520429378860104,
3.71334895258148));
#24291=CARTESIAN_POINT('Ctrl Pts',(6.01993098456861,-0.568156768282506,
3.80000071145885));
#24292=CARTESIAN_POINT('Ctrl Pts',(6.0119783452248,-0.593773517247188,3.89883078914114));
#24293=CARTESIAN_POINT('Ctrl Pts',(6.004025705881,-0.594147126960238,3.99775637428654));
#24294=CARTESIAN_POINT('Ctrl Pts',(5.99607306653719,-0.594520736673288,
4.09668195943193));
#24295=CARTESIAN_POINT('Ctrl Pts',(5.98812042719339,-0.569651207134705,
4.19570305204043));
#24296=CARTESIAN_POINT('Ctrl Pts',(5.98016778784958,-0.52257944308796,4.28271270390554));
#24297=CARTESIAN_POINT('Ctrl Pts',(5.97221514850578,-0.475507679041215,
4.36972235577065));
#24298=CARTESIAN_POINT('Ctrl Pts',(5.96426250916196,-0.406233680486307,
4.44472056689237));
#24299=CARTESIAN_POINT('Ctrl Pts',(5.95630986981816,-0.323226996343023,
4.49853792802592));
#24300=CARTESIAN_POINT('Ctrl Pts',(5.94835723047435,-0.240220312199739,
4.55235528915947));
#24301=CARTESIAN_POINT('Ctrl Pts',(5.94040459113055,-0.143480942468078,
4.58499180030486));
#24302=CARTESIAN_POINT('Ctrl Pts',(5.93245195178675,-0.0448366672808267,
4.59245712746544));
#24303=CARTESIAN_POINT('Ctrl Pts',(5.93124977161035,-0.0299248641651563,
4.59358564190382));
#24304=CARTESIAN_POINT('Ctrl Pts',(5.93004759143396,-0.0149695309183627,
4.59413895459864));
#24305=CARTESIAN_POINT('Ctrl Pts',(5.92884541125757,-1.3134308860685E-5,
4.59412454375027));
#24306=CARTESIAN_POINT('Ctrl Pts',(5.82115458874249,1.31105368646138E-5,
4.59407040741879));
#24307=CARTESIAN_POINT('Ctrl Pts',(5.82645628863475,-0.0659629472043463,
4.59401745734129));
#24308=CARTESIAN_POINT('Ctrl Pts',(5.831757988527,-0.131956164688202,4.58305467757793));
#24309=CARTESIAN_POINT('Ctrl Pts',(5.83705968841925,-0.194280919321303,
4.56148970414564));
#24310=CARTESIAN_POINT('Ctrl Pts',(5.84501232776306,-0.287769103462499,
4.52914187992864));
#24311=CARTESIAN_POINT('Ctrl Pts',(5.85296496710686,-0.373003060391055,
4.47293858298203));
#24312=CARTESIAN_POINT('Ctrl Pts',(5.86091760645067,-0.439561779454174,
4.39975142997742));
#24313=CARTESIAN_POINT('Ctrl Pts',(5.86887024579447,-0.506120498517293,
4.32656427697281));
#24314=CARTESIAN_POINT('Ctrl Pts',(5.87682288513828,-0.554003979714975,
4.2363932679102));
#24315=CARTESIAN_POINT('Ctrl Pts',(5.88477552448209,-0.577357812582609,
4.14026304025204));
#24316=CARTESIAN_POINT('Ctrl Pts',(5.8927281638259,-0.600711645450243,4.04413281259387));
#24317=CARTESIAN_POINT('Ctrl Pts',(5.9006808031697,-0.59953582998783,3.94204336634015));
#24318=CARTESIAN_POINT('Ctrl Pts',(5.90863344251351,-0.573974130801472,
3.84647652011691));
#24319=CARTESIAN_POINT('Ctrl Pts',(5.91658608185731,-0.548412431615114,
3.75090967389367));
#24320=CARTESIAN_POINT('Ctrl Pts',(5.92453872120112,-0.498464848704808,
3.66186542770092));
#24321=CARTESIAN_POINT('Ctrl Pts',(5.93249136054493,-0.430238144626613,
3.59023066587279));
#24322=CARTESIAN_POINT('Ctrl Pts',(5.94044399988873,-0.362011440548417,
3.51859590404466));
#24323=CARTESIAN_POINT('Ctrl Pts',(5.94839663923254,-0.275505615302329,
3.46437062658116));
#24324=CARTESIAN_POINT('Ctrl Pts',(5.95634927857635,-0.181297202577209,
3.43418458862315));
#24325=CARTESIAN_POINT('Ctrl Pts',(5.96430191792015,-0.087088789852092,
3.40399855066514));
#24326=CARTESIAN_POINT('Ctrl Pts',(5.97225455726396,0.0148222103520573,
3.39785175221263));
#24327=CARTESIAN_POINT('Ctrl Pts',(5.98020719660777,0.111975824940657,3.41649576758492));
#24328=CARTESIAN_POINT('Ctrl Pts',(5.98815983595157,0.209129439529257,3.43513978295721));
#24329=CARTESIAN_POINT('Ctrl Pts',(5.99611247529537,0.301525668502307,3.47857461215431));
#24330=CARTESIAN_POINT('Ctrl Pts',(6.00406511463918,0.377867748972965,3.54148967172874));
#24331=CARTESIAN_POINT('Ctrl Pts',(6.01201775398299,0.454209829443624,3.60440473130317));
#24332=CARTESIAN_POINT('Ctrl Pts',(6.0199703933268,0.514497761411887,3.68680002125492));
#24333=CARTESIAN_POINT('Ctrl Pts',(6.02792303267061,0.551360647735685,3.77860175380959));
#24334=CARTESIAN_POINT('Ctrl Pts',(6.03587567201441,0.588223534059482,3.87040348636426));
#24335=CARTESIAN_POINT('Ctrl Pts',(6.04382831135821,0.601661374738811,3.97161166152184));
#24336=CARTESIAN_POINT('Ctrl Pts',(6.05178095070202,0.590030977261751,4.06985190192822));
#24337=CARTESIAN_POINT('Ctrl Pts',(6.05973359004583,0.578400579784692,4.16809214233459));
#24338=CARTESIAN_POINT('Ctrl Pts',(6.06768622938964,0.541701944151245,4.26336444798975));
#24339=CARTESIAN_POINT('Ctrl Pts',(6.07563886873345,0.484422419230229,4.3440210474869));
#24340=CARTESIAN_POINT('Ctrl Pts',(6.08359150807725,0.427142894309213,4.42467764698404));
#24341=CARTESIAN_POINT('Ctrl Pts',(6.09154414742105,0.349282480100627,4.49071854032316));
#24342=CARTESIAN_POINT('Ctrl Pts',(6.09949678676486,0.26035984028865,4.53406826097581));
#24343=CARTESIAN_POINT('Ctrl Pts',(6.10671605409073,0.179637418414302,4.5734203814938));
#24344=CARTESIAN_POINT('Ctrl Pts',(6.11393532141662,0.0897989573399868,
4.59407340590587));
#24345=CARTESIAN_POINT('Ctrl Pts',(6.12115458874249,-9.50793186244619E-6,
4.59413936148612));
#24346=CARTESIAN_POINT('Origin',(4.,0.,4.));
#24347=CARTESIAN_POINT('',(6.52884541125757,2.61457539729726E-5,4.59508370962656));
#24348=CARTESIAN_POINT('',(6.42115458874249,-0.000630941829811112,4.59394485456974));
#24349=CARTESIAN_POINT('',(4.,-7.27562663373442E-17,4.5941));
#24350=CARTESIAN_POINT('Ctrl Pts',(6.52884541125757,2.61457539729726E-5,
4.59508370962656));
#24351=CARTESIAN_POINT('Ctrl Pts',(6.5129582963415,0.196771080344787,4.59506033873941));
#24352=CARTESIAN_POINT('Ctrl Pts',(6.49707118142544,0.393450480974957,4.48779253427891));
#24353=CARTESIAN_POINT('Ctrl Pts',(6.48118406650938,0.500111739713094,4.32240987211318));
#24354=CARTESIAN_POINT('Ctrl Pts',(6.46527878782176,0.606894944490356,4.15683812760557));
#24355=CARTESIAN_POINT('Ctrl Pts',(6.44937350913416,0.623454053851315,3.93301856375293));
#24356=CARTESIAN_POINT('Ctrl Pts',(6.43346823044654,0.541809843535619,3.75368369989414));
#24357=CARTESIAN_POINT('Ctrl Pts',(6.41756295175893,0.460165633219924,3.57434883603535));
#24358=CARTESIAN_POINT('Ctrl Pts',(6.40165767307132,0.280318103227576,3.43949867217041));
#24359=CARTESIAN_POINT('Ctrl Pts',(6.3857523943837,0.085604811340831,3.41110814665827));
#24360=CARTESIAN_POINT('Ctrl Pts',(6.36984711569609,-0.109108480545914,
3.38271762114613));
#24361=CARTESIAN_POINT('Ctrl Pts',(6.35394183700848,-0.318687534327053,
3.46078673398678));
#24362=CARTESIAN_POINT('Ctrl Pts',(6.33803655832087,-0.448733343985475,
3.60951691634857));
#24363=CARTESIAN_POINT('Ctrl Pts',(6.33008391897706,-0.513756248814686,
3.68388200752946));
#24364=CARTESIAN_POINT('Ctrl Pts',(6.32213127963325,-0.558895842613217,
3.77591236609064));
#24365=CARTESIAN_POINT('Ctrl Pts',(6.31417864028945,-0.579995970841135,
3.87270290659392));
#24366=CARTESIAN_POINT('Ctrl Pts',(6.30622600094564,-0.601096099069052,
3.9694934470972));
#24367=CARTESIAN_POINT('Ctrl Pts',(6.29827336160184,-0.598156761726356,
4.07104416954258));
#24368=CARTESIAN_POINT('Ctrl Pts',(6.29032072225803,-0.570614590620327,
4.16591643177432));
#24369=CARTESIAN_POINT('Ctrl Pts',(6.28236808291422,-0.543072419514299,
4.26078869400605));
#24370=CARTESIAN_POINT('Ctrl Pts',(6.27441544357042,-0.490927414644939,
4.34898249602413));
#24371=CARTESIAN_POINT('Ctrl Pts',(6.26646280422661,-0.421087730399527,
4.41916768405122));
#24372=CARTESIAN_POINT('Ctrl Pts',(6.2585101648828,-0.351248046154114,4.48935287207832));
#24373=CARTESIAN_POINT('Ctrl Pts',(6.250557525539,-0.263713682532649,4.54152944611444));
#24374=CARTESIAN_POINT('Ctrl Pts',(6.24260488619519,-0.168899197391682,
4.5696117428605));
#24375=CARTESIAN_POINT('Ctrl Pts',(6.23801839454932,-0.114217245248871,
4.58580752565092));
#24376=CARTESIAN_POINT('Ctrl Pts',(6.23343190290344,-0.0571138332845632,
4.59398924930378));
#24377=CARTESIAN_POINT('Ctrl Pts',(6.22884541125756,-1.27841859475647E-5,
4.5940334609955));
#24378=CARTESIAN_POINT('Ctrl Pts',(6.12115458874249,-9.50793186244619E-6,
4.59413936148612));
#24379=CARTESIAN_POINT('Ctrl Pts',(6.12188796076042,-0.00913273504488762,
4.59414606160884));
#24380=CARTESIAN_POINT('Ctrl Pts',(6.12262133277835,-0.0182556526135436,
4.59394031163173));
#24381=CARTESIAN_POINT('Ctrl Pts',(6.12335470479628,-0.0273686726716501,
4.59352013235631));
#24382=CARTESIAN_POINT('Ctrl Pts',(6.13130734414009,-0.126189680404606,
4.58896373511797));
#24383=CARTESIAN_POINT('Ctrl Pts',(6.13925998348389,-0.223846830455152,
4.55919239267511));
#24384=CARTESIAN_POINT('Ctrl Pts',(6.14721262282769,-0.308403173896691,
4.50784224986958));
#24385=CARTESIAN_POINT('Ctrl Pts',(6.1551652621715,-0.392959517338232,4.45649210706404));
#24386=CARTESIAN_POINT('Ctrl Pts',(6.16311790151532,-0.464415054170765,
4.38356316389581));
#24387=CARTESIAN_POINT('Ctrl Pts',(6.17107054085912,-0.514027768136376,
4.29797916579711));
#24388=CARTESIAN_POINT('Ctrl Pts',(6.17902318020293,-0.563640482101988,
4.2123951676984));
#24389=CARTESIAN_POINT('Ctrl Pts',(6.18697581954673,-0.591410373200678,
4.11415611466921));
#24390=CARTESIAN_POINT('Ctrl Pts',(6.19492845889053,-0.593952774873424,
4.0152594949342));
#24391=CARTESIAN_POINT('Ctrl Pts',(6.20288109823434,-0.59649517654617,3.9163628751992));
#24392=CARTESIAN_POINT('Ctrl Pts',(6.21083373757815,-0.573810088792972,
3.81680868875837));
#24393=CARTESIAN_POINT('Ctrl Pts',(6.21878637692196,-0.528651094032059,
3.72879442104321));
#24394=CARTESIAN_POINT('Ctrl Pts',(6.22673901626577,-0.483492099271145,
3.64078015332805));
#24395=CARTESIAN_POINT('Ctrl Pts',(6.23469165560957,-0.415859197502516,
3.56430580433857));
#24396=CARTESIAN_POINT('Ctrl Pts',(6.24264429495337,-0.334059153459168,
3.50867301156809));
#24397=CARTESIAN_POINT('Ctrl Pts',(6.25059693429718,-0.252259109415819,
3.45304021879761));
#24398=CARTESIAN_POINT('Ctrl Pts',(6.25854957364099,-0.156291923097747,
3.41824898224614));
#24399=CARTESIAN_POINT('Ctrl Pts',(6.2665022129848,-0.057819682214149,3.40864436538418));
#24400=CARTESIAN_POINT('Ctrl Pts',(6.2744548523286,0.0406525586694487,3.39903974852221));
#24401=CARTESIAN_POINT('Ctrl Pts',(6.28240749167241,0.141629854118573,3.41462175134974));
#24402=CARTESIAN_POINT('Ctrl Pts',(6.29036013101621,0.232632044389671,3.453312878872));
#24403=CARTESIAN_POINT('Ctrl Pts',(6.29831277036002,0.323634234660771,3.49200400639426));
#24404=CARTESIAN_POINT('Ctrl Pts',(6.30626540970382,0.404661319753841,3.55380425861124));
#24405=CARTESIAN_POINT('Ctrl Pts',(6.31421804904763,0.466059055789261,3.63148218419904));
#24406=CARTESIAN_POINT('Ctrl Pts',(6.32217068839144,0.527456791824679,3.70916010978684));
#24407=CARTESIAN_POINT('Ctrl Pts',(6.33012332773525,0.569225178802449,3.80271570874544));
#24408=CARTESIAN_POINT('Ctrl Pts',(6.33807596707905,0.585790493249255,3.90010619949006));
#24409=CARTESIAN_POINT('Ctrl Pts',(6.34602860642286,0.602355807696062,3.99749669023468));
#24410=CARTESIAN_POINT('Ctrl Pts',(6.35398124576666,0.593718049611903,4.09872207276531));
#24411=CARTESIAN_POINT('Ctrl Pts',(6.36193388511047,0.56173881546021,4.19248215342453));
#24412=CARTESIAN_POINT('Ctrl Pts',(6.36988652445427,0.529759581308516,4.28624223408375));
#24413=CARTESIAN_POINT('Ctrl Pts',(6.37783916379808,0.474438871089287,4.37253701287156));
#24414=CARTESIAN_POINT('Ctrl Pts',(6.38579180314189,0.401374624788453,4.4390182948332));
#24415=CARTESIAN_POINT('Ctrl Pts',(6.39757939834209,0.293077024234899,4.53755846574697));
#24416=CARTESIAN_POINT('Ctrl Pts',(6.40936699354229,0.145797072855576,4.59256860517148));
#24417=CARTESIAN_POINT('Ctrl Pts',(6.42115458874249,-0.000630941829811112,
4.59394485456974));
#24418=CARTESIAN_POINT('Origin',(4.,0.,4.));
#24419=CARTESIAN_POINT('',(6.82884541125756,0.000528213615369061,4.5937871332276));
#24420=CARTESIAN_POINT('',(6.72115458874249,0.000109070110168276,4.59505938903171));
#24421=CARTESIAN_POINT('',(4.,-7.27562663373442E-17,4.5941));
#24422=CARTESIAN_POINT('Ctrl Pts',(6.82884541125756,0.000528213615369061,
4.5937871332276));
#24423=CARTESIAN_POINT('Ctrl Pts',(6.82429524715479,0.0572034606387535,
4.59426930340541));
#24424=CARTESIAN_POINT('Ctrl Pts',(6.81974508305202,0.113754426020979,4.58681959872387));
#24425=CARTESIAN_POINT('Ctrl Pts',(6.81519491894924,0.167823213394864,4.57092612439125));
#24426=CARTESIAN_POINT('Ctrl Pts',(6.79928964026163,0.356822799356826,4.51536985589957));
#24427=CARTESIAN_POINT('Ctrl Pts',(6.78338436157403,0.515493156338912,4.35664088088147));
#24428=CARTESIAN_POINT('Ctrl Pts',(6.76747908288642,0.570983871223461,4.16762126762428));
#24429=CARTESIAN_POINT('Ctrl Pts',(6.7515738041988,0.626474586108011,3.97860165436708));
#24430=CARTESIAN_POINT('Ctrl Pts',(6.73566852551118,0.578785658895023,3.75929140287077));
#24431=CARTESIAN_POINT('Ctrl Pts',(6.71976324682357,0.449805704301045,3.61038767491097));
#24432=CARTESIAN_POINT('Ctrl Pts',(6.70385796813595,0.320825749707067,3.46148394695116));
#24433=CARTESIAN_POINT('Ctrl Pts',(6.68795268944834,0.110554767732096,3.38298674252784));
#24434=CARTESIAN_POINT('Ctrl Pts',(6.67204741076073,-0.0844443642884844,
3.4109402193496));
#24435=CARTESIAN_POINT('Ctrl Pts',(6.65614213207312,-0.279443496309066,
3.43889369617135));
#24436=CARTESIAN_POINT('Ctrl Pts',(6.64023685338551,-0.459170778375258,
3.57329785423817));
#24437=CARTESIAN_POINT('Ctrl Pts',(6.6243315746979,-0.541132009270427,3.75243704050979));
#24438=CARTESIAN_POINT('Ctrl Pts',(6.60842629601029,-0.623093240165596,
3.9315762267814));
#24439=CARTESIAN_POINT('Ctrl Pts',(6.59252101732267,-0.60728841988974,4.15545044125781));
#24440=CARTESIAN_POINT('Ctrl Pts',(6.57661573863506,-0.500919754058047,
4.32127168369798));
#24441=CARTESIAN_POINT('Ctrl Pts',(6.56069229617589,-0.394429615589227,
4.48728229340579));
#24442=CARTESIAN_POINT('Ctrl Pts',(6.54476885371673,-0.197168666623305,
4.59510713395368));
#24443=CARTESIAN_POINT('Ctrl Pts',(6.52884541125757,2.61457539729726E-5,
4.59508370962656));
#24444=CARTESIAN_POINT('Ctrl Pts',(6.42115458874249,-0.000630941829811112,
4.59394485456974));
#24445=CARTESIAN_POINT('Ctrl Pts',(6.4252722722299,-0.0517816819022344,
4.59442561076518));
#24446=CARTESIAN_POINT('Ctrl Pts',(6.42938995571731,-0.102828462800867,
4.58836159088269));
#24447=CARTESIAN_POINT('Ctrl Pts',(6.43350763920472,-0.152073274319339,
4.5753220992581));
#24448=CARTESIAN_POINT('Ctrl Pts',(6.44941291789233,-0.342290043897387,
4.52495476314113));
#24449=CARTESIAN_POINT('Ctrl Pts',(6.46531819657995,-0.5056209461254,4.37051151428857));
#24450=CARTESIAN_POINT('Ctrl Pts',(6.48122347526756,-0.56632363157735,4.18304963962536));
#24451=CARTESIAN_POINT('Ctrl Pts',(6.49712875395518,-0.627026317029301,
3.99558776496215));
#24452=CARTESIAN_POINT('Ctrl Pts',(6.51303403264279,-0.58510078570519,3.77510726448829));
#24453=CARTESIAN_POINT('Ctrl Pts',(6.5289393113304,-0.460166914262479,3.62276494217392));
#24454=CARTESIAN_POINT('Ctrl Pts',(6.54484459001801,-0.335233042819767,
3.47042261985956));
#24455=CARTESIAN_POINT('Ctrl Pts',(6.56074986870563,-0.127290831258456,
3.38621847570468));
#24456=CARTESIAN_POINT('Ctrl Pts',(6.57665514739324,0.068373869747762,3.4088573345089));
#24457=CARTESIAN_POINT('Ctrl Pts',(6.59256042608085,0.26403857075398,3.43149619331313));
#24458=CARTESIAN_POINT('Ctrl Pts',(6.60846570476847,0.447425761205104,3.56097805507645));
#24459=CARTESIAN_POINT('Ctrl Pts',(6.62437098345608,0.534230294511761,3.73782813427527));
#24460=CARTESIAN_POINT('Ctrl Pts',(6.64027626214369,0.621034827818418,3.91467821347409));
#24461=CARTESIAN_POINT('Ctrl Pts',(6.65618154083131,0.611256703980608,4.1388965101084));
#24462=CARTESIAN_POINT('Ctrl Pts',(6.67208681951892,0.509439333868548,4.30754322537844));
#24463=CARTESIAN_POINT('Ctrl Pts',(6.68799209820653,0.40762196375649,4.47618994064847));
#24464=CARTESIAN_POINT('Ctrl Pts',(6.70389737689414,0.213765347370184,4.58926507455422));
#24465=CARTESIAN_POINT('Ctrl Pts',(6.71980265558175,0.016851802420978,4.59484308232941));
#24466=CARTESIAN_POINT('Ctrl Pts',(6.72025329996867,0.0112726493937942,
4.59500112406784));
#24467=CARTESIAN_POINT('Ctrl Pts',(6.72070394435558,0.00569104238866241,
4.59507287148453));
#24468=CARTESIAN_POINT('Ctrl Pts',(6.72115458874249,0.000109070110168276,
4.59505938903171));
#24469=CARTESIAN_POINT('Origin',(4.,0.,4.));
#24470=CARTESIAN_POINT('',(7.12884541125757,-0.000233413975479213,4.59320261234329));
#24471=CARTESIAN_POINT('',(7.02115458874249,0.000491936389841303,4.5936290357477));
#24472=CARTESIAN_POINT('',(4.,-7.27562663373442E-17,4.5941));
#24473=CARTESIAN_POINT('Ctrl Pts',(7.12884541125757,-0.000233413975479213,
4.59320261234329));
#24474=CARTESIAN_POINT('Ctrl Pts',(7.11972691928047,0.113624805666132,4.59280158872514));
#24475=CARTESIAN_POINT('Ctrl Pts',(7.11060842730338,0.227688545642871,4.56127879346404));
#24476=CARTESIAN_POINT('Ctrl Pts',(7.10148993532628,0.322592019514134,4.50005536307953));
#24477=CARTESIAN_POINT('Ctrl Pts',(7.08558465663867,0.488131036726243,4.39326405099382));
#24478=CARTESIAN_POINT('Ctrl Pts',(7.06967937795105,0.595374147168556,4.19610732087965));
#24479=CARTESIAN_POINT('Ctrl Pts',(7.05377409926343,0.595079946532544,3.99911121186167));
#24480=CARTESIAN_POINT('Ctrl Pts',(7.03786882057582,0.594785745896532,3.80211510284369));
#24481=CARTESIAN_POINT('Ctrl Pts',(7.02196354188821,0.486954234182196,3.60527961492189));
#24482=CARTESIAN_POINT('Ctrl Pts',(7.0060582632006,0.321096900356496,3.49898325846904));
#24483=CARTESIAN_POINT('Ctrl Pts',(6.99015298451299,0.155239566530797,3.3926869020162));
#24484=CARTESIAN_POINT('Ctrl Pts',(6.97424770582538,-0.0686435894062663,
3.37692967703231));
#24485=CARTESIAN_POINT('Ctrl Pts',(6.95834242713776,-0.247754555527299,
3.45894666907189));
#24486=CARTESIAN_POINT('Ctrl Pts',(6.94243714845015,-0.426865521648332,
3.54096366111146));
#24487=CARTESIAN_POINT('Ctrl Pts',(6.92653186976253,-0.561204297953336,
3.72075487017451));
#24488=CARTESIAN_POINT('Ctrl Pts',(6.91062659107492,-0.589088840804576,
3.91576771430201));
#24489=CARTESIAN_POINT('Ctrl Pts',(6.89472131238731,-0.616973383655816,
4.11078055842951));
#24490=CARTESIAN_POINT('Ctrl Pts',(6.8788160336997,-0.538403693053295,4.32101503762147));
#24491=CARTESIAN_POINT('Ctrl Pts',(6.86291075501209,-0.389454440281117,
4.44994049623482));
#24492=CARTESIAN_POINT('Ctrl Pts',(6.85155564042725,-0.283116420949728,
4.54198310574898));
#24493=CARTESIAN_POINT('Ctrl Pts',(6.8402005258424,-0.140907108175025,4.59258385846765));
#24494=CARTESIAN_POINT('Ctrl Pts',(6.82884541125756,0.000528213615369061,
4.5937871332276));
#24495=CARTESIAN_POINT('Ctrl Pts',(6.72115458874249,0.000109070110168276,
4.59505938903171));
#24496=CARTESIAN_POINT('Ctrl Pts',(6.73660922304319,-0.191322006690816,
4.59459701474307));
#24497=CARTESIAN_POINT('Ctrl Pts',(6.75206385734389,-0.38318268672033,4.49389457135631));
#24498=CARTESIAN_POINT('Ctrl Pts',(6.76751849164459,-0.49122657597837,4.33588597251985));
#24499=CARTESIAN_POINT('Ctrl Pts',(6.78342377033221,-0.60242093591639,4.17326997329048));
#24500=CARTESIAN_POINT('Ctrl Pts',(6.79932904901982,-0.624839182280325,
3.94995709318712));
#24501=CARTESIAN_POINT('Ctrl Pts',(6.81523432770743,-0.548195780923551,
3.76848141254984));
#24502=CARTESIAN_POINT('Ctrl Pts',(6.83113960639504,-0.471552379566775,
3.58700573191256));
#24503=CARTESIAN_POINT('Ctrl Pts',(6.84704488508266,-0.295847330489284,
3.44736725074137));
#24504=CARTESIAN_POINT('Ctrl Pts',(6.86295016377027,-0.101752734572189,
3.41368297698799));
#24505=CARTESIAN_POINT('Ctrl Pts',(6.87885544245788,0.0923418613449005,
3.37999870323461));
#24506=CARTESIAN_POINT('Ctrl Pts',(6.8947607211455,0.304826004101594,3.45226863689903));
#24507=CARTESIAN_POINT('Ctrl Pts',(6.91066599983311,0.438133727661537,3.59730899203965));
#24508=CARTESIAN_POINT('Ctrl Pts',(6.92657127852072,0.571441451221483,3.74234934718029));
#24509=CARTESIAN_POINT('Ctrl Pts',(6.94247655720833,0.625572755584675,3.96016012379713));
#24510=CARTESIAN_POINT('Ctrl Pts',(6.95838183589594,0.57567402069499,4.15073208753033));
#24511=CARTESIAN_POINT('Ctrl Pts',(6.97428711458356,0.525775285805305,4.34130405126353));
#24512=CARTESIAN_POINT('Ctrl Pts',(6.99019239327118,0.371846511662747,4.5046372021131));
#24513=CARTESIAN_POINT('Ctrl Pts',(7.00609767195879,0.184564651688987,4.56573572985967));
#24514=CARTESIAN_POINT('Ctrl Pts',(7.01111664422002,0.125467135782336,4.58501560681028));
#24515=CARTESIAN_POINT('Ctrl Pts',(7.01613561648126,0.0630485115161635,
4.59411554829291));
#24516=CARTESIAN_POINT('Ctrl Pts',(7.02115458874249,0.000491936389841303,
4.5936290357477));
#24517=CARTESIAN_POINT('Origin',(4.,0.,4.));
#24518=CARTESIAN_POINT('',(7.42884541125756,-0.000438237927964824,4.59464495791636));
#24519=CARTESIAN_POINT('',(7.32115458874249,-0.000317338366111653,4.59328419319629));
#24520=CARTESIAN_POINT('',(4.,-7.27562663373442E-17,4.5941));
#24521=CARTESIAN_POINT('Ctrl Pts',(7.42884541125756,-0.000438237927964824,
4.59464495791636));
#24522=CARTESIAN_POINT('Ctrl Pts',(7.41515859140615,0.169409178821721,4.5932420274804));
#24523=CARTESIAN_POINT('Ctrl Pts',(7.40147177155473,0.340360224580004,4.51673272682389));
#24524=CARTESIAN_POINT('Ctrl Pts',(7.38778495170331,0.450965110664874,4.38826722161738));
#24525=CARTESIAN_POINT('Ctrl Pts',(7.37187967301569,0.579497637321094,4.23897909740477));
#24526=CARTESIAN_POINT('Ctrl Pts',(7.35597439432808,0.626535888751401,4.01952688559808));
#24527=CARTESIAN_POINT('Ctrl Pts',(7.34006911564046,0.570481892017836,3.83067375781486));
#24528=CARTESIAN_POINT('Ctrl Pts',(7.32416383695285,0.51442789528427,3.64182063003164));
#24529=CARTESIAN_POINT('Ctrl Pts',(7.30825855826524,0.355281650386831,3.48356658627189));
#24530=CARTESIAN_POINT('Ctrl Pts',(7.29235327957763,0.166116376105148,3.42857518785077));
#24531=CARTESIAN_POINT('Ctrl Pts',(7.27644800089002,-0.023048898176535,
3.37358378942964));
#24532=CARTESIAN_POINT('Ctrl Pts',(7.2605427222024,-0.242233201842457,3.42185503634715));
#24533=CARTESIAN_POINT('Ctrl Pts',(7.24463744351479,-0.390796368104757,
3.5512248149675));
#24534=CARTESIAN_POINT('Ctrl Pts',(7.22873216482718,-0.539359534367058,
3.68059459358785));
#24535=CARTESIAN_POINT('Ctrl Pts',(7.21282688613957,-0.617301563225728,
3.89106290391106));
#24536=CARTESIAN_POINT('Ctrl Pts',(7.19692160745195,-0.588834786584626,
4.08599160058025));
#24537=CARTESIAN_POINT('Ctrl Pts',(7.18101632876434,-0.560368009943526,
4.28092029724944));
#24538=CARTESIAN_POINT('Ctrl Pts',(7.16511105007672,-0.425492427802657,
4.46030938026461));
#24539=CARTESIAN_POINT('Ctrl Pts',(7.14920577138911,-0.24613717474127,4.54179097474357));
#24540=CARTESIAN_POINT('Ctrl Pts',(7.1424189846786,-0.169606239833077,4.57655919310821));
#24541=CARTESIAN_POINT('Ctrl Pts',(7.13563219796808,-0.0849767524450092,
4.59350108952231));
#24542=CARTESIAN_POINT('Ctrl Pts',(7.12884541125757,-0.000233413975479213,
4.59320261234329));
#24543=CARTESIAN_POINT('Ctrl Pts',(7.02115458874249,0.000491936389841303,
4.5936290357477));
#24544=CARTESIAN_POINT('Ctrl Pts',(7.03204089516887,-0.135195214358064,
4.59257377495492));
#24545=CARTESIAN_POINT('Ctrl Pts',(7.04292720159524,-0.271531381894462,
4.54641716720817));
#24546=CARTESIAN_POINT('Ctrl Pts',(7.05381350802162,-0.376033620593693,
4.46121547122365));
#24547=CARTESIAN_POINT('Ctrl Pts',(7.06971878670923,-0.528715087097646,
4.33673278019746));
#24548=CARTESIAN_POINT('Ctrl Pts',(7.08562406539685,-0.613443074300594,
4.1289034935015));
#24549=CARTESIAN_POINT('Ctrl Pts',(7.10152934408446,-0.591314251018945,
3.93315398851514));
#24550=CARTESIAN_POINT('Ctrl Pts',(7.11743462277207,-0.569185427737295,
3.73740448352876));
#24551=CARTESIAN_POINT('Ctrl Pts',(7.13333990145968,-0.440199793971044,
3.55373476025198));
#24552=CARTESIAN_POINT('Ctrl Pts',(7.14924518014729,-0.263582002606135,
3.46647820559892));
#24553=CARTESIAN_POINT('Ctrl Pts',(7.16515045883491,-0.0869642112412332,
3.37922165094586));
#24554=CARTESIAN_POINT('Ctrl Pts',(7.18105573752253,0.137285737722324,3.38837826491652));
#24555=CARTESIAN_POINT('Ctrl Pts',(7.19696101621014,0.306201705590428,3.48974370695041));
#24556=CARTESIAN_POINT('Ctrl Pts',(7.21286629489775,0.47511767345854,3.59110914898431));
#24557=CARTESIAN_POINT('Ctrl Pts',(7.22877157358536,0.588699660231196,3.78468341908144));
#24558=CARTESIAN_POINT('Ctrl Pts',(7.24467685227297,0.594795648982816,3.98158540759));
#24559=CARTESIAN_POINT('Ctrl Pts',(7.26058213096058,0.600891637734436,4.17848739609855));
#24560=CARTESIAN_POINT('Ctrl Pts',(7.2764874096482,0.499501628465021,4.37871710301853));
#24561=CARTESIAN_POINT('Ctrl Pts',(7.29239268833581,0.337179610128186,4.49033751492072));
#24562=CARTESIAN_POINT('Ctrl Pts',(7.30197998847137,0.239335998647354,4.5576194790522));
#24563=CARTESIAN_POINT('Ctrl Pts',(7.31156728860693,0.119353510611835,4.59270637405629));
#24564=CARTESIAN_POINT('Ctrl Pts',(7.32115458874249,-0.000317338366111653,
4.59328419319629));
#24565=CARTESIAN_POINT('Origin',(4.,0.,4.));
#24566=CARTESIAN_POINT('',(7.72884541125757,0.000455182276646732,4.59460030787683));
#24567=CARTESIAN_POINT('',(7.62115458874249,-0.000367422317862595,4.59479267874092));
#24568=CARTESIAN_POINT('',(4.,-7.27562663373442E-17,4.5941));
#24569=CARTESIAN_POINT('Ctrl Pts',(7.72884541125757,0.000455182276646732,
4.59460030787683));
#24570=CARTESIAN_POINT('Ctrl Pts',(7.72649554221944,0.0296217258780686,
4.59484761241511));
#24571=CARTESIAN_POINT('Ctrl Pts',(7.72414567318131,0.0587549042441869,
4.59288776399295));
#24572=CARTESIAN_POINT('Ctrl Pts',(7.72179580414318,0.0875427725731367,
4.58860617484604));
#24573=CARTESIAN_POINT('Ctrl Pts',(7.70589052545556,0.282395788279217,4.55962589232715));
#24574=CARTESIAN_POINT('Ctrl Pts',(7.68998524676794,0.461428877889185,4.42427810603975));
#24575=CARTESIAN_POINT('Ctrl Pts',(7.67407996808033,0.542437620895056,4.24470879335187));
#24576=CARTESIAN_POINT('Ctrl Pts',(7.65817468939272,0.623446363900926,4.065139480664));
#24577=CARTESIAN_POINT('Ctrl Pts',(7.64226941070511,0.606430760302702,3.84134864157567));
#24578=CARTESIAN_POINT('Ctrl Pts',(7.6263641320175,0.499203655448083,3.67609156159133));
#24579=CARTESIAN_POINT('Ctrl Pts',(7.61045885332988,0.391976550593464,3.51083448160699));
#24580=CARTESIAN_POINT('Ctrl Pts',(7.59455357464227,0.19453794448245,3.40411116072664));
#24581=CARTESIAN_POINT('Ctrl Pts',(7.57864829595466,-0.00245670798462758,
3.40492443279829));
#24582=CARTESIAN_POINT('Ctrl Pts',(7.56274301726704,-0.199451360451705,
3.40573770486994));
#24583=CARTESIAN_POINT('Ctrl Pts',(7.54683773857943,-0.396002059274846,
3.5140875698936));
#24584=CARTESIAN_POINT('Ctrl Pts',(7.53093245989182,-0.50186103876401,3.68022435377194));
#24585=CARTESIAN_POINT('Ctrl Pts',(7.51502718120421,-0.607720018253171,
3.84636113765028));
#24586=CARTESIAN_POINT('Ctrl Pts',(7.4991219025166,-0.622887278408357,4.07028484038331));
#24587=CARTESIAN_POINT('Ctrl Pts',(7.48321662382898,-0.540398655351294,
4.24917917107494));
#24588=CARTESIAN_POINT('Ctrl Pts',(7.46731134514137,-0.45791003229423,4.42807350176658));
#24589=CARTESIAN_POINT('Ctrl Pts',(7.45140606645375,-0.277765526024924,
4.56193846041682));
#24590=CARTESIAN_POINT('Ctrl Pts',(7.43550078776614,-0.0826798719492015,
4.58930892143267));
#24591=CARTESIAN_POINT('Ctrl Pts',(7.43328232892995,-0.0554694406452989,
4.59312653709876));
#24592=CARTESIAN_POINT('Ctrl Pts',(7.43106387009376,-0.0279683367079049,
4.5948723550368));
#24593=CARTESIAN_POINT('Ctrl Pts',(7.42884541125756,-0.000438237927964824,
4.59464495791636));
#24594=CARTESIAN_POINT('Ctrl Pts',(7.32115458874249,-0.000317338366111653,
4.59328419319629));
#24595=CARTESIAN_POINT('Ctrl Pts',(7.32747256729455,-0.0791797758050172,
4.59366497286126));
#24596=CARTESIAN_POINT('Ctrl Pts',(7.3337905458466,-0.157906876560309,4.57905936436794));
#24597=CARTESIAN_POINT('Ctrl Pts',(7.34010852439865,-0.230073660466993,
4.54880513582638));
#24598=CARTESIAN_POINT('Ctrl Pts',(7.35601380308626,-0.411750885321067,
4.47264122794544));
#24599=CARTESIAN_POINT('Ctrl Pts',(7.37191908177388,-0.551851307624962,
4.29730229529918));
#24600=CARTESIAN_POINT('Ctrl Pts',(7.38782436046149,-0.586046744500155,
4.10329655692985));
#24601=CARTESIAN_POINT('Ctrl Pts',(7.4037296391491,-0.620242181375348,3.90929081856053));
#24602=CARTESIAN_POINT('Ctrl Pts',(7.41963491783671,-0.548532632821828,
3.69661827446815));
#24603=CARTESIAN_POINT('Ctrl Pts',(7.43554019652432,-0.403844087697925,
3.56292915991696));
#24604=CARTESIAN_POINT('Ctrl Pts',(7.45144547521194,-0.259155542574025,
3.42924004536577));
#24605=CARTESIAN_POINT('Ctrl Pts',(7.46735075389955,-0.0414880008797467,
3.37453436035576));
#24606=CARTESIAN_POINT('Ctrl Pts',(7.48325603258717,0.149214809903968,3.42393064079835));
#24607=CARTESIAN_POINT('Ctrl Pts',(7.49916131127478,0.339917620687686,3.47332692124094));
#24608=CARTESIAN_POINT('Ctrl Pts',(7.51506658996239,0.50365570056084,3.62682516713614));
#24609=CARTESIAN_POINT('Ctrl Pts',(7.53097186865001,0.56524745100941,3.81394547807041));
#24610=CARTESIAN_POINT('Ctrl Pts',(7.54687714733762,0.626839201457978,4.00106578900469));
#24611=CARTESIAN_POINT('Ctrl Pts',(7.56278242602523,0.58628462248197,4.22180816497804));
#24612=CARTESIAN_POINT('Ctrl Pts',(7.57868770471284,0.462204660718925,4.3748170457164));
#24613=CARTESIAN_POINT('Ctrl Pts',(7.59284333272272,0.351774041004839,4.51099427596058));
#24614=CARTESIAN_POINT('Ctrl Pts',(7.60699896073261,0.175183620117616,4.59352033541115));
#24615=CARTESIAN_POINT('Ctrl Pts',(7.62115458874249,-0.000367422317862596,
4.59479267874092));
#24616=CARTESIAN_POINT('Origin',(4.,0.,4.));
#24617=CARTESIAN_POINT('',(8.02884541125756,0.000208508845897126,4.59318438507865));
#24618=CARTESIAN_POINT('',(7.92115458874249,0.000504499356536197,4.59443266285439));
#24619=CARTESIAN_POINT('',(4.,-7.27562663373442E-17,4.5941));
#24620=CARTESIAN_POINT('Ctrl Pts',(8.02884541125756,0.000208508845897126,
4.59318438507865));
#24621=CARTESIAN_POINT('Ctrl Pts',(8.02192721434511,0.0865993248636432,
4.5934556945658));
#24622=CARTESIAN_POINT('Ctrl Pts',(8.01500901743265,0.17288466952141,4.57582457789876));
#24623=CARTESIAN_POINT('Ctrl Pts',(8.0080908205202,0.250602156771344,4.53974023855861));
#24624=CARTESIAN_POINT('Ctrl Pts',(7.99218554183259,0.42927852421987,4.4567805482338));
#24625=CARTESIAN_POINT('Ctrl Pts',(7.97628026314498,0.562668370741438,4.27628395749428));
#24626=CARTESIAN_POINT('Ctrl Pts',(7.96037498445736,0.589524722071826,4.08112686462655));
#24627=CARTESIAN_POINT('Ctrl Pts',(7.94446970576975,0.616381073402214,3.88596977175883));
#24628=CARTESIAN_POINT('Ctrl Pts',(7.92856442708213,0.536703929541425,3.67615217676291));
#24629=CARTESIAN_POINT('Ctrl Pts',(7.91265914839452,0.387077664089382,3.54801344261061));
#24630=CARTESIAN_POINT('Ctrl Pts',(7.89675386970691,0.237451398637336,3.41987470845831));
#24631=CARTESIAN_POINT('Ctrl Pts',(7.88084859101929,0.0178760115940344,
3.37341483514963));
#24632=CARTESIAN_POINT('Ctrl Pts',(7.86494331233168,-0.170828768780714,
3.42996623095257));
#24633=CARTESIAN_POINT('Ctrl Pts',(7.84903803364407,-0.359533549155462,
3.48651762675552));
#24634=CARTESIAN_POINT('Ctrl Pts',(7.83313275495647,-0.517367722861657,
3.64608029167009));
#24635=CARTESIAN_POINT('Ctrl Pts',(7.81722747626885,-0.571860514742998,
3.83538980050754));
#24636=CARTESIAN_POINT('Ctrl Pts',(7.80132219758124,-0.626353306624339,
4.02469930934499));
#24637=CARTESIAN_POINT('Ctrl Pts',(7.78541691889362,-0.577504716680827,
4.24375566210532));
#24638=CARTESIAN_POINT('Ctrl Pts',(7.769511640206,-0.447743950807975,4.3919774491103));
#24639=CARTESIAN_POINT('Ctrl Pts',(7.75595623055652,-0.337154229471824,
4.51830073342946));
#24640=CARTESIAN_POINT('Ctrl Pts',(7.74240082090705,-0.16779438404434,4.593173711641));
#24641=CARTESIAN_POINT('Ctrl Pts',(7.72884541125757,0.000455182276646732,
4.59460030787683));
#24642=CARTESIAN_POINT('Ctrl Pts',(7.62115458874249,-0.000367422317862596,
4.59479267874092));
#24643=CARTESIAN_POINT('Ctrl Pts',(7.62290423942022,-0.022065717876263,
4.59494994172972));
#24644=CARTESIAN_POINT('Ctrl Pts',(7.62465389009795,-0.043748134618359,
4.59386587358433));
#24645=CARTESIAN_POINT('Ctrl Pts',(7.62640354077568,-0.0652877816099521,
4.59148835294282));
#24646=CARTESIAN_POINT('Ctrl Pts',(7.64230881946329,-0.261094917625702,
4.56987539392751));
#24647=CARTESIAN_POINT('Ctrl Pts',(7.6582140981509,-0.445103845107109,4.44137409039354));
#24648=CARTESIAN_POINT('Ctrl Pts',(7.67411937683852,-0.532825449416136,
4.2649868044631));
#24649=CARTESIAN_POINT('Ctrl Pts',(7.69002465552613,-0.620547053725161,
4.08859951853267));
#24650=CARTESIAN_POINT('Ctrl Pts',(7.70592993421374,-0.611981334861803,
3.86432625020577));
#24651=CARTESIAN_POINT('Ctrl Pts',(7.72183521290136,-0.511061308497056,
3.69514379608856));
#24652=CARTESIAN_POINT('Ctrl Pts',(7.73774049158897,-0.410141282132307,
3.52596134197134));
#24653=CARTESIAN_POINT('Ctrl Pts',(7.75364577027658,-0.216866948266163,
3.4118697020638));
#24654=CARTESIAN_POINT('Ctrl Pts',(7.76955104896419,-0.0199817042712483,
3.40525493058698));
#24655=CARTESIAN_POINT('Ctrl Pts',(7.78545632765181,0.176903539723664,3.39864015911017));
#24656=CARTESIAN_POINT('Ctrl Pts',(7.80136160633942,0.377399693847348,3.49950225606407));
#24657=CARTESIAN_POINT('Ctrl Pts',(7.81726688502703,0.489447406431712,3.66152961365368));
#24658=CARTESIAN_POINT('Ctrl Pts',(7.83317216371464,0.601495119016078,3.82355697124329));
#24659=CARTESIAN_POINT('Ctrl Pts',(7.84907744240226,0.625094390061116,4.04674958946861));
#24660=CARTESIAN_POINT('Ctrl Pts',(7.86498272108987,0.549409432699027,4.22862686054007));
#24661=CARTESIAN_POINT('Ctrl Pts',(7.88088799977748,0.473724475336938,4.41050413161152));
#24662=CARTESIAN_POINT('Ctrl Pts',(7.89679327846509,0.298755289567731,4.55106605552911));
#24663=CARTESIAN_POINT('Ctrl Pts',(7.91269855715271,0.104840323164387,4.58577254351526));
#24664=CARTESIAN_POINT('Ctrl Pts',(7.9155172343493,0.0704753991278659,4.59192310448195));
#24665=CARTESIAN_POINT('Ctrl Pts',(7.91833591154589,0.0355154700816755,
4.59474920414003));
#24666=CARTESIAN_POINT('Ctrl Pts',(7.92115458874249,0.000504499356536197,
4.59443266285439));
#24667=CARTESIAN_POINT('Origin',(4.,0.,4.));
#24668=CARTESIAN_POINT('',(8.32884541125757,-0.000534402448739424,4.5938336238991));
#24669=CARTESIAN_POINT('',(8.2211545887425,0.000116005647334215,4.59313666129657));
#24670=CARTESIAN_POINT('',(4.,-7.27562663373442E-17,4.5941));
#24671=CARTESIAN_POINT('Ctrl Pts',(8.32884541125757,-0.000534402448739424,
4.5938336238991));
#24672=CARTESIAN_POINT('Ctrl Pts',(8.31735888647079,0.142509087977489,4.59259298046846));
#24673=CARTESIAN_POINT('Ctrl Pts',(8.30587236168401,0.286359812054371,4.54070236535691));
#24674=CARTESIAN_POINT('Ctrl Pts',(8.29438583689723,0.393155811111917,4.44670960845581));
#24675=CARTESIAN_POINT('Ctrl Pts',(8.27848055820962,0.541035187969857,4.31655875596735));
#24676=CARTESIAN_POINT('Ctrl Pts',(8.262575279522,0.617867056310918,4.10568264439756));
#24677=CARTESIAN_POINT('Ctrl Pts',(8.24667000083439,0.588373472681163,3.91090666274675));
#24678=CARTESIAN_POINT('Ctrl Pts',(8.23076472214677,0.558879889051408,3.71613068109593));
#24679=CARTESIAN_POINT('Ctrl Pts',(8.21485944345917,0.423060853450833,3.53745482936408));
#24680=CARTESIAN_POINT('Ctrl Pts',(8.19895416477155,0.243278720997716,3.45691949951456));
#24681=CARTESIAN_POINT('Ctrl Pts',(8.18304888608394,0.0634965885445972,
3.37638416966503));
#24682=CARTESIAN_POINT('Ctrl Pts',(8.16714360739632,-0.160248640761069,
3.39398936169784));
#24683=CARTESIAN_POINT('Ctrl Pts',(8.15123832870871,-0.325222623502191,
3.50165151624576));
#24684=CARTESIAN_POINT('Ctrl Pts',(8.1353330500211,-0.490196606243315,3.60931367079368));
#24685=CARTESIAN_POINT('Ctrl Pts',(8.11942777133349,-0.59639934241989,3.80703278785672));
#24686=CARTESIAN_POINT('Ctrl Pts',(8.10352249264588,-0.595067028646789,
4.00402461368555));
#24687=CARTESIAN_POINT('Ctrl Pts',(8.08761721395827,-0.593734714873688,
4.20101643951437));
#24688=CARTESIAN_POINT('Ctrl Pts',(8.07171193527065,-0.484867351150922,
4.39728097410898));
#24689=CARTESIAN_POINT('Ctrl Pts',(8.05580665658303,-0.3184522251018,4.50270184645125));
#24690=CARTESIAN_POINT('Ctrl Pts',(8.04681957480788,-0.224421408301879,
4.56226861162124));
#24691=CARTESIAN_POINT('Ctrl Pts',(8.03783249303272,-0.112017456676448,
4.59283194056482));
#24692=CARTESIAN_POINT('Ctrl Pts',(8.02884541125756,0.000208508845897126,
4.59318438507865));
#24693=CARTESIAN_POINT('Ctrl Pts',(7.92115458874249,0.000504499356536197,
4.59443266285439));
#24694=CARTESIAN_POINT('Ctrl Pts',(7.93424119023351,-0.162045019349314,
4.59296301969496));
#24695=CARTESIAN_POINT('Ctrl Pts',(7.94732779172453,-0.325694779556815,
4.52375140444135));
#24696=CARTESIAN_POINT('Ctrl Pts',(7.96041439321555,-0.436005268305889,
4.40499428651169));
#24697=CARTESIAN_POINT('Ctrl Pts',(7.97631967190316,-0.570075146335334,
4.26065848946726));
#24698=CARTESIAN_POINT('Ctrl Pts',(7.99222495059077,-0.625354155356748,
4.04313584332371));
#24699=CARTESIAN_POINT('Ctrl Pts',(8.00813022927838,-0.576460513088508,
3.85230354456612));
#24700=CARTESIAN_POINT('Ctrl Pts',(8.024035507966,-0.527566870820267,3.66147124580852));
#24701=CARTESIAN_POINT('Ctrl Pts',(8.03994078665361,-0.374500577262366,
3.49732929443689));
#24702=CARTESIAN_POINT('Ctrl Pts',(8.05584606534123,-0.187543198716277,
3.43524473024767));
#24703=CARTESIAN_POINT('Ctrl Pts',(8.07175134402884,-0.000585820170193818,
3.37316016605846));
#24704=CARTESIAN_POINT('Ctrl Pts',(8.08765662271645,0.220262643364076,3.41313298905166));
#24705=CARTESIAN_POINT('Ctrl Pts',(8.10356190140406,0.37359792075985,3.53680937001953));
#24706=CARTESIAN_POINT('Ctrl Pts',(8.11946718009167,0.526933198155627,3.66048575098741));
#24707=CARTESIAN_POINT('Ctrl Pts',(8.13537245877928,0.612755289412907,3.86786568992997));
#24708=CARTESIAN_POINT('Ctrl Pts',(8.1512777374669,0.591658321059451,4.06372909240644));
#24709=CARTESIAN_POINT('Ctrl Pts',(8.16718301615451,0.570561352705995,4.2595924948829));
#24710=CARTESIAN_POINT('Ctrl Pts',(8.18308829484212,0.44254532474181,4.44393936089328));
#24711=CARTESIAN_POINT('Ctrl Pts',(8.19899357352974,0.266389781296621,4.53212540863836));
#24712=CARTESIAN_POINT('Ctrl Pts',(8.20638057860065,0.184576572093718,4.57308230066594));
#24713=CARTESIAN_POINT('Ctrl Pts',(8.21376758367158,0.0923795717789203,
4.59329710918813));
#24714=CARTESIAN_POINT('Ctrl Pts',(8.2211545887425,0.000116005647334215,
4.59313666129657));
#24715=CARTESIAN_POINT('Origin',(4.,0.,4.));
#24716=CARTESIAN_POINT('',(8.62884541125757,3.48566139269993E-5,4.59507810043999));
#24717=CARTESIAN_POINT('',(8.5211545887425,-0.000547905086566465,4.594005652201));
#24718=CARTESIAN_POINT('',(4.,-7.27562663373442E-17,4.5941));
#24719=CARTESIAN_POINT('Ctrl Pts',(8.62884541125757,3.48566139269993E-5,
4.59507810043999));
#24720=CARTESIAN_POINT('Ctrl Pts',(8.62869583728408,0.00188744051982823,
4.59507966949126));
#24721=CARTESIAN_POINT('Ctrl Pts',(8.62854626331059,0.00374001065808006,
4.59507176912216));
#24722=CARTESIAN_POINT('Ctrl Pts',(8.6283966893371,0.00559249142073073,
4.59505435897699));
#24723=CARTESIAN_POINT('Ctrl Pts',(8.61249141064948,0.202580123064263,4.59320301275402));
#24724=CARTESIAN_POINT('Ctrl Pts',(8.59658613196187,0.398557131004382,4.48381890612783));
#24725=CARTESIAN_POINT('Ctrl Pts',(8.58068085327426,0.503539164298441,4.31712659320126));
#24726=CARTESIAN_POINT('Ctrl Pts',(8.56477557458664,0.608521197592498,4.15043428027469));
#24727=CARTESIAN_POINT('Ctrl Pts',(8.54887029589904,0.622508256240502,3.92643376104774));
#24728=CARTESIAN_POINT('Ctrl Pts',(8.53296501721142,0.539078074654942,3.74797659726896));
#24729=CARTESIAN_POINT('Ctrl Pts',(8.51705973852381,0.455647893069379,3.56951943349019));
#24730=CARTESIAN_POINT('Ctrl Pts',(8.50115445983619,0.274800471250253,3.43660562515959));
#24731=CARTESIAN_POINT('Ctrl Pts',(8.48524918114857,0.0795732942734406,
3.41026356994308));
#24732=CARTESIAN_POINT('Ctrl Pts',(8.46934390246096,-0.115653882703369,
3.38392151472657));
#24733=CARTESIAN_POINT('Ctrl Pts',(8.45343862377335,-0.32526081483786,3.46415121262414));
#24734=CARTESIAN_POINT('Ctrl Pts',(8.43753334508574,-0.453004866631874,
3.61411458059983));
#24735=CARTESIAN_POINT('Ctrl Pts',(8.42162806639813,-0.580748918425883,
3.76407794857552));
#24736=CARTESIAN_POINT('Ctrl Pts',(8.40572278771052,-0.626630089879422,
3.98377498662932));
#24737=CARTESIAN_POINT('Ctrl Pts',(8.3898175090229,-0.569581688133314,4.17233010950212));
#24738=CARTESIAN_POINT('Ctrl Pts',(8.37391223033529,-0.512533286387202,
4.36088523237493));
#24739=CARTESIAN_POINT('Ctrl Pts',(8.35800695164768,-0.352555311441432,
4.51829844006673));
#24740=CARTESIAN_POINT('Ctrl Pts',(8.34210167296007,-0.163102881281137,
4.57229224720906));
#24741=CARTESIAN_POINT('Ctrl Pts',(8.33768291905923,-0.110469810133188,
4.58729263485501));
#24742=CARTESIAN_POINT('Ctrl Pts',(8.3332641651584,-0.0555618361628184,
4.59431088730997));
#24743=CARTESIAN_POINT('Ctrl Pts',(8.32884541125757,-0.000534402448739424,
4.5938336238991));
#24744=CARTESIAN_POINT('Ctrl Pts',(8.2211545887425,0.000116005647334215,
4.59313666129657));
#24745=CARTESIAN_POINT('Ctrl Pts',(8.22967286235919,-0.106277085140544,
4.59295164192424));
#24746=CARTESIAN_POINT('Ctrl Pts',(8.23819113597589,-0.212758691085218,
4.56567285125378));
#24747=CARTESIAN_POINT('Ctrl Pts',(8.24670940959258,-0.303508593564514,
4.51186277431583));
#24748=CARTESIAN_POINT('Ctrl Pts',(8.26261468828019,-0.472956366054245,
4.41138886276846));
#24749=CARTESIAN_POINT('Ctrl Pts',(8.2785199669678,-0.587556852107514,4.21841581019395));
#24750=CARTESIAN_POINT('Ctrl Pts',(8.29442524565541,-0.594690356875377,
4.02154867831793));
#24751=CARTESIAN_POINT('Ctrl Pts',(8.31033052434302,-0.60182386164324,3.82468154644191));
#24752=CARTESIAN_POINT('Ctrl Pts',(8.32623580303064,-0.501490385125681,
3.62392033526436));
#24753=CARTESIAN_POINT('Ctrl Pts',(8.34214108171825,-0.339758814980244,
3.51144609945163));
#24754=CARTESIAN_POINT('Ctrl Pts',(8.35804636040587,-0.178027244834812,
3.3989718636389));
#24755=CARTESIAN_POINT('Ctrl Pts',(8.37395163909348,0.0451024189384938,
3.37478460319097));
#24756=CARTESIAN_POINT('Ctrl Pts',(8.38985691778109,0.227178474572579,3.44999008482693));
#24757=CARTESIAN_POINT('Ctrl Pts',(8.4057621964687,0.40925453020667,3.5251955664629));
#24758=CARTESIAN_POINT('Ctrl Pts',(8.42166747515631,0.550276977701535,3.69979379018275));
#24759=CARTESIAN_POINT('Ctrl Pts',(8.43757275384392,0.585494275335268,3.89361663829603));
#24760=CARTESIAN_POINT('Ctrl Pts',(8.45347803253154,0.620711572969,4.0874394864093));
#24761=CARTESIAN_POINT('Ctrl Pts',(8.46938331121915,0.550123720741606,4.30048695891599));
#24762=CARTESIAN_POINT('Ctrl Pts',(8.48528858990677,0.406141674070155,4.4349366697363));
#24763=CARTESIAN_POINT('Ctrl Pts',(8.49724392285201,0.297916389879728,4.53599689564107));
#24764=CARTESIAN_POINT('Ctrl Pts',(8.50919925579725,0.148224117540273,4.59265016978245));
#24765=CARTESIAN_POINT('Ctrl Pts',(8.5211545887425,-0.000547905086566465,
4.594005652201));
#24766=CARTESIAN_POINT('Origin',(4.,0.,4.));
#24767=CARTESIAN_POINT('',(8.92884541125757,0.000516595407308196,4.59372894893997));
#24768=CARTESIAN_POINT('',(8.82115458874249,0.000142235148737217,4.59503945166131));
#24769=CARTESIAN_POINT('',(4.,-7.27562663373442E-17,4.5941));
#24770=CARTESIAN_POINT('Ctrl Pts',(8.92884541125757,0.000516595407308196,
4.59372894893997));
#24771=CARTESIAN_POINT('Ctrl Pts',(8.92412750940976,0.0592956068199462,
4.59421507565108));
#24772=CARTESIAN_POINT('Ctrl Pts',(8.91940960756194,0.117944888069788,4.58619493689145));
#24773=CARTESIAN_POINT('Ctrl Pts',(8.91469170571413,0.17383025386194,4.56912565303288));
#24774=CARTESIAN_POINT('Ctrl Pts',(8.89878642702651,0.362234410233906,4.51158064138869));
#24775=CARTESIAN_POINT('Ctrl Pts',(8.8828811483389,0.519225559109383,4.35118846702123));
#24776=CARTESIAN_POINT('Ctrl Pts',(8.86697586965128,0.572720006672535,4.16159443076672));
#24777=CARTESIAN_POINT('Ctrl Pts',(8.85107059096367,0.626214454235688,3.97200039451221));
#24778=CARTESIAN_POINT('Ctrl Pts',(8.83516531227606,0.576212200486512,3.75320449637065));
#24779=CARTESIAN_POINT('Ctrl Pts',(8.81926003358845,0.445672164925724,3.60566855627755));
#24780=CARTESIAN_POINT('Ctrl Pts',(8.80335475490084,0.315132129364936,3.45813261618446));
#24781=CARTESIAN_POINT('Ctrl Pts',(8.78744947621322,0.104054311992536,3.38185663413984));
#24782=CARTESIAN_POINT('Ctrl Pts',(8.77154419752561,-0.0906432834200916,
3.41186331412789));
#24783=CARTESIAN_POINT('Ctrl Pts',(8.755638918838,-0.285340878832719,3.44186999411594));
#24784=CARTESIAN_POINT('Ctrl Pts',(8.73973364015038,-0.463658252285575,
3.57815933613666));
#24785=CARTESIAN_POINT('Ctrl Pts',(8.72382836146277,-0.543719609875046,
3.75815304026071));
#24786=CARTESIAN_POINT('Ctrl Pts',(8.70792308277515,-0.623780967464517,
3.93814674438476));
#24787=CARTESIAN_POINT('Ctrl Pts',(8.69201780408754,-0.605586309190603,
4.16184481061213));
#24788=CARTESIAN_POINT('Ctrl Pts',(8.67611252539993,-0.497489852380174,
4.32653455081593));
#24789=CARTESIAN_POINT('Ctrl Pts',(8.66035682068581,-0.390409939629295,
4.48967554111606));
#24790=CARTESIAN_POINT('Ctrl Pts',(8.64460111597169,-0.195111159088962,
4.59491282095998));
#24791=CARTESIAN_POINT('Ctrl Pts',(8.62884541125757,3.48566139269993E-5,
4.59507810043999));
#24792=CARTESIAN_POINT('Ctrl Pts',(8.5211545887425,-0.000547905086566465,
4.594005652201));
#24793=CARTESIAN_POINT('Ctrl Pts',(8.52510453448487,-0.0497009834700827,
4.59445349267793));
#24794=CARTESIAN_POINT('Ctrl Pts',(8.52905448022724,-0.0987536084630192,
4.58886509038946));
#24795=CARTESIAN_POINT('Ctrl Pts',(8.53300442596961,-0.146177075786514,
4.57684766499685));
#24796=CARTESIAN_POINT('Ctrl Pts',(8.54890970465722,-0.337137537856201,
4.52845700030318));
#24797=CARTESIAN_POINT('Ctrl Pts',(8.56481498334483,-0.501682220880061,
4.37582372178193));
#24798=CARTESIAN_POINT('Ctrl Pts',(8.58072026203244,-0.564259167724997,
4.18903057354857));
#24799=CARTESIAN_POINT('Ctrl Pts',(8.59662554072005,-0.626836114569933,
4.00223742531521));
#24800=CARTESIAN_POINT('Ctrl Pts',(8.61253081940767,-0.587445325235947,
3.78128440736974));
#24801=CARTESIAN_POINT('Ctrl Pts',(8.62843609809528,-0.464173383698336,
3.62762379780141));
#24802=CARTESIAN_POINT('Ctrl Pts',(8.6443413767829,-0.340901442160722,3.47396318823307));
#24803=CARTESIAN_POINT('Ctrl Pts',(8.66024665547051,-0.133748348419481,
3.38759498704188));
#24804=CARTESIAN_POINT('Ctrl Pts',(8.67615193415812,0.0621699608040676,
3.40817581827756));
#24805=CARTESIAN_POINT('Ctrl Pts',(8.69205721284573,0.25808827002761,3.42875664951325));
#24806=CARTESIAN_POINT('Ctrl Pts',(8.70796249153334,0.44277179473346,3.55628651317581));
#24807=CARTESIAN_POINT('Ctrl Pts',(8.72386777022095,0.531421673692279,3.73220909121499));
#24808=CARTESIAN_POINT('Ctrl Pts',(8.73977304890857,0.620071552651101,3.90813166925417));
#24809=CARTESIAN_POINT('Ctrl Pts',(8.75567832759618,0.612687785862888,4.13244696166997));
#24810=CARTESIAN_POINT('Ctrl Pts',(8.7715836062838,0.512660686655375,4.30215887618246));
#24811=CARTESIAN_POINT('Ctrl Pts',(8.78748888497141,0.412633587447865,4.47187079069495));
#24812=CARTESIAN_POINT('Ctrl Pts',(8.80339416365902,0.21996315582106,4.58697932730413));
#24813=CARTESIAN_POINT('Ctrl Pts',(8.81929944234663,0.0231155027642346,
4.59463151583965));
#24814=CARTESIAN_POINT('Ctrl Pts',(8.81991782447859,0.0154622529370322,
4.59492902566351));
#24815=CARTESIAN_POINT('Ctrl Pts',(8.82053620661054,0.00780268890311657,
4.59506410656044));
#24816=CARTESIAN_POINT('Ctrl Pts',(8.82115458874249,0.000142235148737217,
4.59503945166131));
#24817=CARTESIAN_POINT('Origin',(4.,0.,4.));
#24818=CARTESIAN_POINT('',(9.22884541125756,-0.000264402795292107,4.59322887297718));
#24819=CARTESIAN_POINT('',(9.12115458874249,0.000475196148639644,4.59357609051269));
#24820=CARTESIAN_POINT('',(4.,-7.27562663373442E-17,4.5941));
#24821=CARTESIAN_POINT('Ctrl Pts',(9.22884541125756,-0.000264402795292107,
4.59322887297718));
#24822=CARTESIAN_POINT('Ctrl Pts',(9.21955918153543,0.115675446261185,4.59276508993807));
#24823=CARTESIAN_POINT('Ctrl Pts',(9.21027295181329,0.231857423975292,4.55999255403315));
#24824=CARTESIAN_POINT('Ctrl Pts',(9.20098672209116,0.327844211240712,4.49662776730038));
#24825=CARTESIAN_POINT('Ctrl Pts',(9.18508144340355,0.492248565587605,4.38809775866155));
#24826=CARTESIAN_POINT('Ctrl Pts',(9.16917616471593,0.597407924103304,4.18982173958679));
#24827=CARTESIAN_POINT('Ctrl Pts',(9.15327088602831,0.595037558282966,3.99283966966863));
#24828=CARTESIAN_POINT('Ctrl Pts',(9.1373656073407,0.592667192462628,3.79585759975047));
#24829=CARTESIAN_POINT('Ctrl Pts',(9.12146032865309,0.482767102306254,3.60016947898891));
#24830=CARTESIAN_POINT('Ctrl Pts',(9.10555504996548,0.315798759724268,3.49562701355602));
#24831=CARTESIAN_POINT('Ctrl Pts',(9.08964977127787,0.148830417142278,3.39108454812312));
#24832=CARTESIAN_POINT('Ctrl Pts',(9.07374449259025,-0.0752061778653251,
3.37768773801888));
#24833=CARTESIAN_POINT('Ctrl Pts',(9.05783921390264,-0.253442899077741,
3.46158783167087));
#24834=CARTESIAN_POINT('Ctrl Pts',(9.04193393521502,-0.431679620290152,
3.54548792532286));
#24835=CARTESIAN_POINT('Ctrl Pts',(9.02602865652741,-0.56411646770738,3.72668492273107));
#24836=CARTESIAN_POINT('Ctrl Pts',(9.0101233778398,-0.589944043936388,3.92198082849844));
#24837=CARTESIAN_POINT('Ctrl Pts',(8.99421809915219,-0.615771620165397,
4.11727673426582));
#24838=CARTESIAN_POINT('Ctrl Pts',(8.97831282046457,-0.534989925206181,
4.32667154839236));
#24839=CARTESIAN_POINT('Ctrl Pts',(8.96240754177696,-0.384690495792338,
4.45402003099517));
#24840=CARTESIAN_POINT('Ctrl Pts',(8.95122016493716,-0.278973620993485,
4.54359378149875));
#24841=CARTESIAN_POINT('Ctrl Pts',(8.94003278809737,-0.138863784294423,
4.59257621560968));
#24842=CARTESIAN_POINT('Ctrl Pts',(8.92884541125757,0.000516595407308196,
4.59372894893997));
#24843=CARTESIAN_POINT('Ctrl Pts',(8.82115458874249,0.000142235148737217,
4.59503945166131));
#24844=CARTESIAN_POINT('Ctrl Pts',(8.83644148529816,-0.189230254871984,
4.59442996300828));
#24845=CARTESIAN_POINT('Ctrl Pts',(8.85172838185382,-0.379146468724227,
4.49620311855542));
#24846=CARTESIAN_POINT('Ctrl Pts',(8.86701527840948,-0.487657002993039,
4.34104488491935));
#24847=CARTESIAN_POINT('Ctrl Pts',(8.88292055709709,-0.600556981206626,
4.17961022500168));
#24848=CARTESIAN_POINT('Ctrl Pts',(8.89882583578469,-0.62533206314696,3.95654506470448));
#24849=CARTESIAN_POINT('Ctrl Pts',(8.91473111447231,-0.550606579334316,
3.77427148852754));
#24850=CARTESIAN_POINT('Ctrl Pts',(8.93063639315992,-0.47588109552167,3.5919979123506));
#24851=CARTESIAN_POINT('Ctrl Pts',(8.94654167184753,-0.301655045956043,
3.45051592029392));
#24852=CARTESIAN_POINT('Ctrl Pts',(8.96244695053515,-0.107925661701669,
3.41478805750048));
#24853=CARTESIAN_POINT('Ctrl Pts',(8.97835222922276,0.0858037225526985,
3.37906019470703));
#24854=CARTESIAN_POINT('Ctrl Pts',(8.99425750791037,0.299036441495806,3.4490864611768));
#24855=CARTESIAN_POINT('Ctrl Pts',(9.01016278659798,0.433865051721373,3.5927137579139));
#24856=CARTESIAN_POINT('Ctrl Pts',(9.0260680652856,0.568693661946943,3.736341054651));
#24857=CARTESIAN_POINT('Ctrl Pts',(9.04197334397321,0.625118163454969,3.95356938165542));
#24858=CARTESIAN_POINT('Ctrl Pts',(9.05787862266082,0.577230812276762,4.14465668133936));
#24859=CARTESIAN_POINT('Ctrl Pts',(9.07378390134844,0.529343461098555,4.3357439810233));
#24860=CARTESIAN_POINT('Ctrl Pts',(9.08968918003605,0.377144257234124,4.50069025338676));
#24861=CARTESIAN_POINT('Ctrl Pts',(9.10559445872366,0.190516636080703,4.56375914846174));
#24862=CARTESIAN_POINT('Ctrl Pts',(9.11078116872994,0.129657384941762,4.58432590969837));
#24863=CARTESIAN_POINT('Ctrl Pts',(9.11596787873622,0.0651369761893139,
4.59405891310139));
#24864=CARTESIAN_POINT('Ctrl Pts',(9.12115458874249,0.000475196148639644,
4.59357609051269));
#24865=CARTESIAN_POINT('Origin',(4.,0.,4.));
#24866=CARTESIAN_POINT('',(9.52884541125756,-0.000414715089906426,4.59470005288553));
#24867=CARTESIAN_POINT('',(9.4211545887425,-0.000345133784900094,4.59331940772745));
#24868=CARTESIAN_POINT('',(4.,-7.27562663373442E-17,4.5941));
#24869=CARTESIAN_POINT('Ctrl Pts',(9.52884541125756,-0.000414715089906426,
4.59470005288553));
#24870=CARTESIAN_POINT('Ctrl Pts',(9.5149908536611,0.17147269131647,4.59333531965569));
#24871=CARTESIAN_POINT('Ctrl Pts',(9.50113629606464,0.344448366351018,4.51470554290992));
#24872=CARTESIAN_POINT('Ctrl Pts',(9.48728173846818,0.455032043431697,4.38349290156166));
#24873=CARTESIAN_POINT('Ctrl Pts',(9.47137645978057,0.581984072756561,4.23285845412795));
#24874=CARTESIAN_POINT('Ctrl Pts',(9.45547118109296,0.626706888961734,4.01292269047354));
#24875=CARTESIAN_POINT('Ctrl Pts',(9.43956590240535,0.56866566691212,3.82467080855373));
#24876=CARTESIAN_POINT('Ctrl Pts',(9.42366062371773,0.510624444862503,3.63641892663391));
#24877=CARTESIAN_POINT('Ctrl Pts',(9.40775534503012,0.349819184558098,3.47985092644869));
#24878=CARTESIAN_POINT('Ctrl Pts',(9.39185006634251,0.160084858421151,3.42685620983728));
#24879=CARTESIAN_POINT('Ctrl Pts',(9.37594478765489,-0.0296494677157886,
3.37386149322587));
#24880=CARTESIAN_POINT('Ctrl Pts',(9.36003950896728,-0.248312859685263,
3.42444006018826));
#24881=CARTESIAN_POINT('Ctrl Pts',(9.34413423027966,-0.395504338780113,
3.55536837257802));
#24882=CARTESIAN_POINT('Ctrl Pts',(9.32822895159205,-0.542695817874971,
3.6862966849678));
#24883=CARTESIAN_POINT('Ctrl Pts',(9.31232367290444,-0.618415384095196,
3.89757474278496));
#24884=CARTESIAN_POINT('Ctrl Pts',(9.29641839421683,-0.587895816063128,
4.09219260031737));
#24885=CARTESIAN_POINT('Ctrl Pts',(9.28051311552922,-0.55737624803106,4.28681045784976));
#24886=CARTESIAN_POINT('Ctrl Pts',(9.26460783684159,-0.42061754574671,4.4647681150974));
#24887=CARTESIAN_POINT('Ctrl Pts',(9.24870255815398,-0.240413519515492,
4.54435494461976));
#24888=CARTESIAN_POINT('Ctrl Pts',(9.24208350918851,-0.165420852186184,
4.57747534017911));
#24889=CARTESIAN_POINT('Ctrl Pts',(9.23546446022304,-0.0829041350566004,
4.59355944875842));
#24890=CARTESIAN_POINT('Ctrl Pts',(9.22884541125756,-0.000264402795292107,
4.59322887297718));
#24891=CARTESIAN_POINT('Ctrl Pts',(9.12115458874249,0.000475196148639644,
4.59357609051269));
#24892=CARTESIAN_POINT('Ctrl Pts',(9.13187315742383,-0.133151270259641,
4.59257831599443));
#24893=CARTESIAN_POINT('Ctrl Pts',(9.14259172610516,-0.267381477949042,
4.54795275857003));
#24894=CARTESIAN_POINT('Ctrl Pts',(9.1533102947865,-0.371151898503526,4.46515291500219));
#24895=CARTESIAN_POINT('Ctrl Pts',(9.16921557347411,-0.525136773491911,
4.34228626868117));
#24896=CARTESIAN_POINT('Ctrl Pts',(9.18512085216173,-0.612050485026272,
4.13536145825263));
#24897=CARTESIAN_POINT('Ctrl Pts',(9.20102613084934,-0.591985933785934,
3.93938960239856));
#24898=CARTESIAN_POINT('Ctrl Pts',(9.21693140953695,-0.571921382545595,
3.74341774654449));
#24899=CARTESIAN_POINT('Ctrl Pts',(9.23283668822456,-0.444878568530549,
3.55839884526489));
#24900=CARTESIAN_POINT('Ctrl Pts',(9.24874196691217,-0.269190177198291,
3.46928575052316));
#24901=CARTESIAN_POINT('Ctrl Pts',(9.26464724559978,-0.0935017858660342,
3.38017265578144));
#24902=CARTESIAN_POINT('Ctrl Pts',(9.28055252428739,0.130832182783434,3.38696536757758));
#24903=CARTESIAN_POINT('Ctrl Pts',(9.29645780297501,0.300807061133818,3.48654496003073));
#24904=CARTESIAN_POINT('Ctrl Pts',(9.31236308166262,0.470781939484206,3.58612455248389));
#24905=CARTESIAN_POINT('Ctrl Pts',(9.32826836035024,0.586397727535503,3.77849102559406));
#24906=CARTESIAN_POINT('Ctrl Pts',(9.34417363903785,0.594568546715174,3.97531783326339));
#24907=CARTESIAN_POINT('Ctrl Pts',(9.36007891772546,0.602739365894845,4.17214464093271));
#24908=CARTESIAN_POINT('Ctrl Pts',(9.37598419641307,0.503465216202894,4.37343178316119));
#24909=CARTESIAN_POINT('Ctrl Pts',(9.39188947510069,0.342328587234952,4.48675671999422));
#24910=CARTESIAN_POINT('Ctrl Pts',(9.40164451298129,0.243500144778355,4.55626125828842));
#24911=CARTESIAN_POINT('Ctrl Pts',(9.41139955086189,0.121401365174849,4.59267772446372));
#24912=CARTESIAN_POINT('Ctrl Pts',(9.4211545887425,-0.000345133784900094,
4.59331940772745));
#24913=CARTESIAN_POINT('Origin',(4.,0.,4.));
#24914=CARTESIAN_POINT('',(9.82884541125756,0.000474857175501747,4.59454166667424));
#24915=CARTESIAN_POINT('',(9.7211545887425,-0.000338423355870402,4.59484023865297));
#24916=CARTESIAN_POINT('',(4.,-7.27562663373442E-17,4.5941));
#24917=CARTESIAN_POINT('Ctrl Pts',(9.82884541125756,0.000474857175501747,
4.59454166667424));
#24918=CARTESIAN_POINT('Ctrl Pts',(9.82632780447438,0.0317313679687054,
4.59481419231428));
#24919=CARTESIAN_POINT('Ctrl Pts',(9.82381019769121,0.0629485386443197,
4.59256288124703));
#24920=CARTESIAN_POINT('Ctrl Pts',(9.82129259090804,0.093741277189286,4.58765086492638));
#24921=CARTESIAN_POINT('Ctrl Pts',(9.80538731222043,0.288278045752977,4.55661862072519));
#24922=CARTESIAN_POINT('Ctrl Pts',(9.78948203353282,0.465874751366426,4.41939150759219));
#24923=CARTESIAN_POINT('Ctrl Pts',(9.77357675484521,0.54498650030893,4.23897841027765));
#24924=CARTESIAN_POINT('Ctrl Pts',(9.7576714761576,0.624098249251433,4.05856531296313));
#24925=CARTESIAN_POINT('Ctrl Pts',(9.74176619746998,0.604725041522997,3.83496623146707));
#24926=CARTESIAN_POINT('Ctrl Pts',(9.72586091878237,0.495762234499694,3.67084840431546));
#24927=CARTESIAN_POINT('Ctrl Pts',(9.70995564009475,0.386799427476386,3.50673057716384));
#24928=CARTESIAN_POINT('Ctrl Pts',(9.69405036140714,0.188247021158209,3.40209400435668));
#24929=CARTESIAN_POINT('Ctrl Pts',(9.67814508271953,-0.00872811953311764,
3.40498337331868));
#24930=CARTESIAN_POINT('Ctrl Pts',(9.66223980403192,-0.205703260224436,
3.40787274228067));
#24931=CARTESIAN_POINT('Ctrl Pts',(9.6463345253443,-0.4011011352889,3.51828805301183));
#24932=CARTESIAN_POINT('Ctrl Pts',(9.63042924665669,-0.505203307099277,
3.68553126611098));
#24933=CARTESIAN_POINT('Ctrl Pts',(9.61452396796908,-0.609305478909656,
3.85277447921013));
#24934=CARTESIAN_POINT('Ctrl Pts',(9.59861868928147,-0.622111947465945,
4.07684559467727));
#24935=CARTESIAN_POINT('Ctrl Pts',(9.58271341059386,-0.537742524204099,
4.25486063595701));
#24936=CARTESIAN_POINT('Ctrl Pts',(9.56680813190624,-0.453373100942255,
4.43287567723675));
#24937=CARTESIAN_POINT('Ctrl Pts',(9.55090285321863,-0.271827785862281,
4.5648346443291));
#24938=CARTESIAN_POINT('Ctrl Pts',(9.53499757453102,-0.0764645071000137,
4.59014756226876));
#24939=CARTESIAN_POINT('Ctrl Pts',(9.53294685343987,-0.0512756623106346,
4.5934112419387));
#24940=CARTESIAN_POINT('Ctrl Pts',(9.53089613234871,-0.025857110284879,
4.59490205769144));
#24941=CARTESIAN_POINT('Ctrl Pts',(9.52884541125756,-0.000414715089906426,
4.59470005288553));
#24942=CARTESIAN_POINT('Ctrl Pts',(9.4211545887425,-0.000345133784900094,
4.59331940772745));
#24943=CARTESIAN_POINT('Ctrl Pts',(9.42730482954951,-0.0771024252662454,
4.59372396859559));
#24944=CARTESIAN_POINT('Ctrl Pts',(9.43345507035652,-0.153719688677923,
4.57990840728947));
#24945=CARTESIAN_POINT('Ctrl Pts',(9.43960531116353,-0.224276981305518,
4.55119942103951));
#24946=CARTESIAN_POINT('Ctrl Pts',(9.45551058985114,-0.406746812634079,
4.47695445381419));
#24947=CARTESIAN_POINT('Ctrl Pts',(9.47141586853875,-0.548687367047265,
4.30310178792596));
#24948=CARTESIAN_POINT('Ctrl Pts',(9.48732114722636,-0.58492554696818,4.10946721245096));
#24949=CARTESIAN_POINT('Ctrl Pts',(9.50322642591398,-0.621163726889096,
3.91583263697596));
#24950=CARTESIAN_POINT('Ctrl Pts',(9.5191317046016,-0.55169953231774,3.70241615191419));
#24951=CARTESIAN_POINT('Ctrl Pts',(9.53503698328921,-0.408427982613559,
3.56720957829912));
#24952=CARTESIAN_POINT('Ctrl Pts',(9.55094226197682,-0.265156432909381,
3.43200300468405));
#24953=CARTESIAN_POINT('Ctrl Pts',(9.56684754066442,-0.0480775280723801,
3.37500634251568));
#24954=CARTESIAN_POINT('Ctrl Pts',(9.58275281935204,0.14313528264739,3.42239004773181));
#24955=CARTESIAN_POINT('Ctrl Pts',(9.59865809803965,0.334348093367161,3.46977375294793));
#24956=CARTESIAN_POINT('Ctrl Pts',(9.61456337672728,0.499694809969701,3.62153782554855));
#24957=CARTESIAN_POINT('Ctrl Pts',(9.63046865541489,0.563255215433827,3.80799862400389));
#24958=CARTESIAN_POINT('Ctrl Pts',(9.6463739341025,0.626815620897955,3.99445942245922));
#24959=CARTESIAN_POINT('Ctrl Pts',(9.6622792127901,0.588589715223662,4.21561694676927));
#24960=CARTESIAN_POINT('Ctrl Pts',(9.67818449147771,0.466129217091882,4.36992501817411));
#24961=CARTESIAN_POINT('Ctrl Pts',(9.69250785723264,0.355848439261942,4.50888586187125));
#24962=CARTESIAN_POINT('Ctrl Pts',(9.70683122298757,0.177255492135987,4.59363345408847));
#24963=CARTESIAN_POINT('Ctrl Pts',(9.7211545887425,-0.000338423355870402,
4.59484023865297));
#24964=CARTESIAN_POINT('Origin',(4.,0.,4.));
#24965=CARTESIAN_POINT('',(10.1288454112576,0.000175993811045716,4.59316417414361));
#24966=CARTESIAN_POINT('',(10.0211545887425,0.000517772199431355,4.59437035498519));
#24967=CARTESIAN_POINT('',(4.,-7.27562663373442E-17,4.5941));
#24968=CARTESIAN_POINT('Ctrl Pts',(10.1288454112576,0.000175993811045716,
4.59316417414361));
#24969=CARTESIAN_POINT('Ctrl Pts',(10.1217594766001,0.0886689559287146,
4.59339827721605));
#24970=CARTESIAN_POINT('Ctrl Pts',(10.1146735419426,0.177068724884878,4.57486525982572));
#24971=CARTESIAN_POINT('Ctrl Pts',(10.1075876072851,0.256276603526552,4.53706914692868));
#24972=CARTESIAN_POINT('Ctrl Pts',(10.0916823285975,0.434068729046268,4.45223097977176));
#24973=CARTESIAN_POINT('Ctrl Pts',(10.0757770499098,0.565548899719798,4.27033860735548));
#24974=CARTESIAN_POINT('Ctrl Pts',(10.0598717712222,0.590346983641159,4.0749093118617));
#24975=CARTESIAN_POINT('Ctrl Pts',(10.0439664925346,0.61514506756252,3.87948001636793));
#24976=CARTESIAN_POINT('Ctrl Pts',(10.028061213847,0.533261064731712,3.67051379779667));
#24977=CARTESIAN_POINT('Ctrl Pts',(10.0121559351594,0.382292645022166,3.5439591030842));
#24978=CARTESIAN_POINT('Ctrl Pts',(9.99625065647179,0.231324225312614,3.41740440837173));
#24979=CARTESIAN_POINT('Ctrl Pts',(9.98034537778417,0.011271388724311,3.37326123751805));
#24980=CARTESIAN_POINT('Ctrl Pts',(9.96444009909655,-0.17682691184915,3.43179826703564));
#24981=CARTESIAN_POINT('Ctrl Pts',(9.94853482040894,-0.364925212422603,
3.49033529655323));
#24982=CARTESIAN_POINT('Ctrl Pts',(9.93262954172133,-0.521068976981223,
3.65155252644206));
#24983=CARTESIAN_POINT('Ctrl Pts',(9.91672426303372,-0.573563594737602,
3.84142582527571));
#24984=CARTESIAN_POINT('Ctrl Pts',(9.90081898434611,-0.626058212493981,
4.03129912410937));
#24985=CARTESIAN_POINT('Ctrl Pts',(9.8849137056585,-0.574903683448118,4.24982849188785));
#24986=CARTESIAN_POINT('Ctrl Pts',(9.86900842697089,-0.443588003168223,
4.39667448814241));
#24987=CARTESIAN_POINT('Ctrl Pts',(9.85562075506645,-0.333057953489513,
4.52027659892262));
#24988=CARTESIAN_POINT('Ctrl Pts',(9.842233083162,-0.165735336637852,4.59309247934331));
#24989=CARTESIAN_POINT('Ctrl Pts',(9.82884541125756,0.000474857175501747,
4.59454166667424));
#24990=CARTESIAN_POINT('Ctrl Pts',(9.7211545887425,-0.000338423355870402,
4.59484023865297));
#24991=CARTESIAN_POINT('Ctrl Pts',(9.72273650167518,-0.0199523965301825,
4.59497351934566));
#24992=CARTESIAN_POINT('Ctrl Pts',(9.72431841460787,-0.0395541838993478,
4.59408780127083));
#24993=CARTESIAN_POINT('Ctrl Pts',(9.72590032754056,-0.0590504136254521,
4.592143576127));
#24994=CARTESIAN_POINT('Ctrl Pts',(9.74180560622817,-0.255074455621757,
4.57259544417541));
#24995=CARTESIAN_POINT('Ctrl Pts',(9.75771088491579,-0.4404274490251,4.4460405617726));
#24996=CARTESIAN_POINT('Ctrl Pts',(9.7736161636034,-0.530003140903138,4.2705875768224));
#24997=CARTESIAN_POINT('Ctrl Pts',(9.78952144229101,-0.619578832781174,
4.0951345918722));
#24998=CARTESIAN_POINT('Ctrl Pts',(9.80542672097862,-0.61337722313391,3.87078350437461));
#24999=CARTESIAN_POINT('Ctrl Pts',(9.82133199966623,-0.514245828742901,
3.70054684219675));
#25000=CARTESIAN_POINT('Ctrl Pts',(9.83723727835384,-0.41511443435189,3.53031018001889));
#25001=CARTESIAN_POINT('Ctrl Pts',(9.85314255704146,-0.223053255217129,
3.41418794316076));
#25002=CARTESIAN_POINT('Ctrl Pts',(9.86904783572907,-0.0262486593588972,
3.40549855006092));
#25003=CARTESIAN_POINT('Ctrl Pts',(9.88495311441669,0.170555936499329,3.39680915696108));
#25004=CARTESIAN_POINT('Ctrl Pts',(9.9008583931043,0.372103949081026,3.49555260761951));
#25005=CARTESIAN_POINT('Ctrl Pts',(9.91676367179191,0.485853057801912,3.65639008698476));
#25006=CARTESIAN_POINT('Ctrl Pts',(9.93266895047952,0.5996021665228,3.81722756635002));
#25007=CARTESIAN_POINT('Ctrl Pts',(9.94857422916713,0.625552371382872,4.04015907442209));
#25008=CARTESIAN_POINT('Ctrl Pts',(9.96447950785475,0.551788436173011,4.22282389414861));
#25009=CARTESIAN_POINT('Ctrl Pts',(9.98038478654236,0.478024500963153,4.40548871387512));
#25010=CARTESIAN_POINT('Ctrl Pts',(9.99629006522997,0.304546425683368,4.54788684525607));
#25011=CARTESIAN_POINT('Ctrl Pts',(10.0121953439176,0.111008003250015,4.58463509072946));
#25012=CARTESIAN_POINT('Ctrl Pts',(10.0151817588592,0.0746687445744621,
4.59153503329043));
#25013=CARTESIAN_POINT('Ctrl Pts',(10.0181681738009,0.0376222632219309,
4.59471031472953));
#25014=CARTESIAN_POINT('Ctrl Pts',(10.0211545887425,0.000517772199431355,
4.59437035498519));
#25015=CARTESIAN_POINT('Origin',(4.,0.,4.));
#25016=CARTESIAN_POINT('',(10.4288454112576,-0.000541293539476018,4.59389423388278));
#25017=CARTESIAN_POINT('',(10.3211545887425,8.19078234495683E-5,4.59312629593825));
#25018=CARTESIAN_POINT('',(4.,-7.27562663373442E-17,4.5941));
#25019=CARTESIAN_POINT('Ctrl Pts',(10.4288454112576,-0.000541293539476018,
4.59389423388278));
#25020=CARTESIAN_POINT('Ctrl Pts',(10.4171911487257,0.144553461780974,4.59260897165526));
#25021=CARTESIAN_POINT('Ctrl Pts',(10.4055368861939,0.290497422953868,4.53904330389552));
#25022=CARTESIAN_POINT('Ctrl Pts',(10.3938826236621,0.397841883685798,4.4425412994096));
#25023=CARTESIAN_POINT('Ctrl Pts',(10.3779773449745,0.544341377656434,4.31083916286766));
#25024=CARTESIAN_POINT('Ctrl Pts',(10.3620720662869,0.618946539098701,4.09916502578488));
#25025=CARTESIAN_POINT('Ctrl Pts',(10.3461667875993,0.587401834162399,3.90471069671543));
#25026=CARTESIAN_POINT('Ctrl Pts',(10.3302615089117,0.555857129226098,3.710256367646));
#25027=CARTESIAN_POINT('Ctrl Pts',(10.314356230224,0.418162557911234,3.5330218465899));
#25028=CARTESIAN_POINT('Ctrl Pts',(10.2984509515364,0.237541641988682,3.45438572744188));
#25029=CARTESIAN_POINT('Ctrl Pts',(10.2825456728488,0.0569207260661262,
3.37574960829385));
#25030=CARTESIAN_POINT('Ctrl Pts',(10.2666403941612,-0.16662653446412,3.3957118910539));
#25031=CARTESIAN_POINT('Ctrl Pts',(10.2507351154736,-0.330456695071223,
3.50510674001315));
#25032=CARTESIAN_POINT('Ctrl Pts',(10.234829836786,-0.494286855678321,3.61450158897239));
#25033=CARTESIAN_POINT('Ctrl Pts',(10.2189245580984,-0.59839991636228,3.81332900413083));
#25034=CARTESIAN_POINT('Ctrl Pts',(10.2030192794108,-0.594991564317383,
4.01029584814195));
#25035=CARTESIAN_POINT('Ctrl Pts',(10.1871140007231,-0.591583212272486,
4.20726269215308));
#25036=CARTESIAN_POINT('Ctrl Pts',(10.1712087220355,-0.480653447498727,
4.40236896501689));
#25037=CARTESIAN_POINT('Ctrl Pts',(10.1553034433479,-0.313136524928893,
4.50603012050002));
#25038=CARTESIAN_POINT('Ctrl Pts',(10.1464840993178,-0.220249792163878,
4.56350936438632));
#25039=CARTESIAN_POINT('Ctrl Pts',(10.1376647552877,-0.109964716607974,
4.59287280319057));
#25040=CARTESIAN_POINT('Ctrl Pts',(10.1288454112576,0.000175993811045716,
4.59316417414361));
#25041=CARTESIAN_POINT('Ctrl Pts',(10.0211545887425,0.000517772199431355,
4.59437035498519));
#25042=CARTESIAN_POINT('Ctrl Pts',(10.0340734524885,-0.159991692577292,
4.59289973094197));
#25043=CARTESIAN_POINT('Ctrl Pts',(10.0469923162344,-0.321586704601994,
4.52564765365589));
#25044=CARTESIAN_POINT('Ctrl Pts',(10.0599111799804,-0.431712787135162,
4.40956688772629));
#25045=CARTESIAN_POINT('Ctrl Pts',(10.075816458668,-0.567296385500051,4.2666520796839));
#25046=CARTESIAN_POINT('Ctrl Pts',(10.0917217373556,-0.624864812642908,
4.04972410403331));
#25047=CARTESIAN_POINT('Ctrl Pts',(10.1076270160433,-0.577985082339038,
3.85838710972745));
#25048=CARTESIAN_POINT('Ctrl Pts',(10.1235322947309,-0.531105352035168,
3.6670501154216));
#25049=CARTESIAN_POINT('Ctrl Pts',(10.1394375734185,-0.379777464284567,
3.50130410246047));
#25050=CARTESIAN_POINT('Ctrl Pts',(10.1553428521061,-0.193484782987353,
3.43725262786029));
#25051=CARTESIAN_POINT('Ctrl Pts',(10.1712481307937,-0.00719210169012799,
3.37320115326011));
#25052=CARTESIAN_POINT('Ctrl Pts',(10.1871534094813,0.214065373153706,3.41084421702088));
#25053=CARTESIAN_POINT('Ctrl Pts',(10.2030586881689,0.368695569727689,3.53289771681035));
#25054=CARTESIAN_POINT('Ctrl Pts',(10.2189639668565,0.523325766301663,3.65495121659981));
#25055=CARTESIAN_POINT('Ctrl Pts',(10.2348692455442,0.611328684605784,3.86141515241798));
#25056=CARTESIAN_POINT('Ctrl Pts',(10.2507745242318,0.592297107651237,4.05749001970593));
#25057=CARTESIAN_POINT('Ctrl Pts',(10.2666798029194,0.573265530696689,4.25356488699388));
#25058=CARTESIAN_POINT('Ctrl Pts',(10.282585081607,0.447199458483466,4.43925068575162));
#25059=CARTESIAN_POINT('Ctrl Pts',(10.2984903602946,0.271983097956201,4.5292883529079));
#25060=CARTESIAN_POINT('Ctrl Pts',(10.3060451031106,0.188758241169316,4.57205474716445));
#25061=CARTESIAN_POINT('Ctrl Pts',(10.3135998459265,0.0944446272328244,
4.59324204311815));
#25062=CARTESIAN_POINT('Ctrl Pts',(10.3211545887425,8.19078234495684E-5,
4.59312629593825));
#25063=CARTESIAN_POINT('Origin',(4.,0.,4.));
#25064=CARTESIAN_POINT('',(10.7288454112576,7.37317986114466E-5,4.59506942345298));
#25065=CARTESIAN_POINT('',(10.6211545887425,-0.000548317120500629,4.59406879148573));
#25066=CARTESIAN_POINT('',(4.,-7.27562663373442E-17,4.5941));
#25067=CARTESIAN_POINT('Ctrl Pts',(10.7288454112576,7.37317986114466E-5,
4.59506942345298));
#25068=CARTESIAN_POINT('Ctrl Pts',(10.728528099539,0.00400402563557926,
4.59507627971693));
#25069=CARTESIAN_POINT('Ctrl Pts',(10.7282107878205,0.00793419209028873,
4.59504072157671));
#25070=CARTESIAN_POINT('Ctrl Pts',(10.727893476102,0.0118635052742893,4.59496237136513));
#25071=CARTESIAN_POINT('Ctrl Pts',(10.7119881974144,0.208820685209451,4.59103505989901));
#25072=CARTESIAN_POINT('Ctrl Pts',(10.6960829187267,0.403634001393415,4.47959161118634));
#25073=CARTESIAN_POINT('Ctrl Pts',(10.6801776400391,0.506853420906232,4.31180214209248));
#25074=CARTESIAN_POINT('Ctrl Pts',(10.6642723613515,0.610072840419052,4.14401267299861));
#25075=CARTESIAN_POINT('Ctrl Pts',(10.6483670826639,0.621698363260717,3.91987718352354));
#25076=CARTESIAN_POINT('Ctrl Pts',(10.6324618039763,0.536392041177647,3.74230920804366));
#25077=CARTESIAN_POINT('Ctrl Pts',(10.6165565252887,0.451085719094577,3.56474123256377));
#25078=CARTESIAN_POINT('Ctrl Pts',(10.6006512466011,0.26884755208677,3.43374077107907));
#25079=CARTESIAN_POINT('Ctrl Pts',(10.5847459679135,0.0733535965831807,
3.40945769333085));
#25080=CARTESIAN_POINT('Ctrl Pts',(10.5688406892258,-0.122140358920403,
3.38517461558263));
#25081=CARTESIAN_POINT('Ctrl Pts',(10.5529354105382,-0.33089010291977,3.46760892157089));
#25082=CARTESIAN_POINT('Ctrl Pts',(10.5370301318506,-0.457046584443773,
3.61891026549369));
#25083=CARTESIAN_POINT('Ctrl Pts',(10.521124853163,-0.583203065967777,3.7702116094165));
#25084=CARTESIAN_POINT('Ctrl Pts',(10.5052195744754,-0.626766285016417,
3.99037999127385));
#25085=CARTESIAN_POINT('Ctrl Pts',(10.4893142957878,-0.567733854410369,
4.17832340467295));
#25086=CARTESIAN_POINT('Ctrl Pts',(10.4734090171002,-0.508701423804317,
4.36626681807206));
#25087=CARTESIAN_POINT('Ctrl Pts',(10.4575037384126,-0.347073343543565,
4.52198526301292));
#25088=CARTESIAN_POINT('Ctrl Pts',(10.4415984597249,-0.157062390163684,
4.57397941748279));
#25089=CARTESIAN_POINT('Ctrl Pts',(10.4373474435692,-0.106278015462724,
4.58787593542499));
#25090=CARTESIAN_POINT('Ctrl Pts',(10.4330964274134,-0.0534661480554494,
4.59436304694399));
#25091=CARTESIAN_POINT('Ctrl Pts',(10.4288454112576,-0.000541293539476018,
4.59389423388278));
#25092=CARTESIAN_POINT('Ctrl Pts',(10.3211545887425,8.19078234495684E-5,
4.59312629593825));
#25093=CARTESIAN_POINT('Ctrl Pts',(10.3295051246142,-0.104220686264852,
4.59299835631127));
#25094=CARTESIAN_POINT('Ctrl Pts',(10.3378556604858,-0.208583275928277,
4.56684300569277));
#25095=CARTESIAN_POINT('Ctrl Pts',(10.3462061963575,-0.298097175589899,
4.5150330474864));
#25096=CARTESIAN_POINT('Ctrl Pts',(10.3621114750451,-0.468594439767441,
4.41635053935381));
#25097=CARTESIAN_POINT('Ctrl Pts',(10.3780167537327,-0.585222319281217,
4.22459598753381));
#25098=CARTESIAN_POINT('Ctrl Pts',(10.3939220324203,-0.594430225977177,
4.02781496975607));
#25099=CARTESIAN_POINT('Ctrl Pts',(10.4098273111079,-0.603638132673137,
3.83103395197833));
#25100=CARTESIAN_POINT('Ctrl Pts',(10.4257325897955,-0.505426066551287,
3.62922646824286));
#25101=CARTESIAN_POINT('Ctrl Pts',(10.4416378684831,-0.344888853364916,
3.51505397731042));
#25102=CARTESIAN_POINT('Ctrl Pts',(10.4575431471707,-0.184351640178541,
3.40088148637798));
#25103=CARTESIAN_POINT('Ctrl Pts',(10.4734484258584,0.0385107200723601,
3.37434398824859));
#25104=CARTESIAN_POINT('Ctrl Pts',(10.489353704546,0.221369260089487,3.4476263793543));
#25105=CARTESIAN_POINT('Ctrl Pts',(10.5052589832336,0.40422780010661,3.52090877046001));
#25106=CARTESIAN_POINT('Ctrl Pts',(10.5211642619212,0.54708251988996,3.69401105080081));
#25107=CARTESIAN_POINT('Ctrl Pts',(10.5370695406088,0.584340575799814,3.88745197659776));
#25108=CARTESIAN_POINT('Ctrl Pts',(10.5529748192964,0.621598631709669,4.08089290239472));
#25109=CARTESIAN_POINT('Ctrl Pts',(10.568880097984,0.55326002374602,4.29467247364782));
#25110=CARTESIAN_POINT('Ctrl Pts',(10.5847853766716,0.4107029495177,4.43063215550545));
#25111=CARTESIAN_POINT('Ctrl Pts',(10.5969084473619,0.302045344566967,4.53426120008624));
#25112=CARTESIAN_POINT('Ctrl Pts',(10.6090315180522,0.150270129189204,4.59268036842864));
#25113=CARTESIAN_POINT('Ctrl Pts',(10.6211545887425,-0.000548317120500629,
4.59406879148573));
#25114=CARTESIAN_POINT('Origin',(4.,0.,4.));
#25115=CARTESIAN_POINT('',(11.0288454112576,0.000503618959454472,4.59367252935801));
#25116=CARTESIAN_POINT('',(10.9211545887425,0.000179316795020235,4.59501533910171));
#25117=CARTESIAN_POINT('',(4.,-7.27562663373442E-17,4.5941));
#25118=CARTESIAN_POINT('Ctrl Pts',(11.0288454112576,0.000503618959454472,
4.59367252935801));
#25119=CARTESIAN_POINT('Ctrl Pts',(11.0239597716647,0.0613870506829751,
4.59415995979602));
#25120=CARTESIAN_POINT('Ctrl Pts',(11.0190741320719,0.122135879976345,4.58554712933309));
#25121=CARTESIAN_POINT('Ctrl Pts',(11.014188492479,0.179818659528701,4.56726203449827));
#25122=CARTESIAN_POINT('Ctrl Pts',(10.9982832137914,0.36760588100072,4.50773461262244));
#25123=CARTESIAN_POINT('Ctrl Pts',(10.9823779351038,0.52289792528528,4.34569680405454));
#25124=CARTESIAN_POINT('Ctrl Pts',(10.9664726564162,0.574391255511512,4.15554951523459));
#25125=CARTESIAN_POINT('Ctrl Pts',(10.9505673777285,0.625884585737745,3.96540222641464));
#25126=CARTESIAN_POINT('Ctrl Pts',(10.9346620990409,0.573579201905647,3.74714545734266));
#25127=CARTESIAN_POINT('Ctrl Pts',(10.9187568203533,0.441491523412615,3.60099348269406));
#25128=CARTESIAN_POINT('Ctrl Pts',(10.9028515416657,0.309403844919578,3.45484150804546));
#25129=CARTESIAN_POINT('Ctrl Pts',(10.8869462629781,0.0975338717655902,
3.38079432782024));
#25130=CARTESIAN_POINT('Ctrl Pts',(10.8710409842905,-0.0968366678563846,
3.41285127449999));
#25131=CARTESIAN_POINT('Ctrl Pts',(10.8551357056029,-0.291207207478354,
3.44490822117975));
#25132=CARTESIAN_POINT('Ctrl Pts',(10.8392304269153,-0.468078313568319,
3.58306929476445));
#25133=CARTESIAN_POINT('Ctrl Pts',(10.8233251482276,-0.546238257009186,
3.76389677537701));
#25134=CARTESIAN_POINT('Ctrl Pts',(10.80741986954,-0.624398200450053,3.94472425598957));
#25135=CARTESIAN_POINT('Ctrl Pts',(10.7915145908524,-0.603846981241821,
4.16821814362997));
#25136=CARTESIAN_POINT('Ctrl Pts',(10.7756093121648,-0.494020849794526,
4.33175950034039));
#25137=CARTESIAN_POINT('Ctrl Pts',(10.7600213451957,-0.386385759396791,
4.49203819249975));
#25138=CARTESIAN_POINT('Ctrl Pts',(10.7444333782267,-0.193002309618558,
4.59473260886404));
#25139=CARTESIAN_POINT('Ctrl Pts',(10.7288454112576,7.37317986114466E-5,
4.59506942345298));
#25140=CARTESIAN_POINT('Ctrl Pts',(10.6211545887425,-0.000548317120500629,
4.59406879148573));
#25141=CARTESIAN_POINT('Ctrl Pts',(10.6249367967398,-0.0476013079303647,
4.5945019577127));
#25142=CARTESIAN_POINT('Ctrl Pts',(10.6287190047372,-0.0945611723716044,
4.58938408097059));
#25143=CARTESIAN_POINT('Ctrl Pts',(10.6325012127345,-0.140089514783682,
4.57835619988505));
#25144=CARTESIAN_POINT('Ctrl Pts',(10.6484064914221,-0.331549364363767,
4.53198076994489));
#25145=CARTESIAN_POINT('Ctrl Pts',(10.6643117701097,-0.497693523030948,
4.38109011760241));
#25146=CARTESIAN_POINT('Ctrl Pts',(10.6802170487973,-0.562235622104956,
4.19496684675621));
#25147=CARTESIAN_POINT('Ctrl Pts',(10.6961223274849,-0.626777721178965,
4.00884357591002));
#25148=CARTESIAN_POINT('Ctrl Pts',(10.7120276061725,-0.589717760659791,
3.78748768656011));
#25149=CARTESIAN_POINT('Ctrl Pts',(10.7279328848602,-0.468072106540212,
3.63253643830059));
#25150=CARTESIAN_POINT('Ctrl Pts',(10.7438381635478,-0.346426452420629,
3.47758519004106));
#25151=CARTESIAN_POINT('Ctrl Pts',(10.7597434422354,-0.140195104700642,
3.38903858287192));
#25152=CARTESIAN_POINT('Ctrl Pts',(10.775648720923,0.0559292266755373,3.40755347270721));
#25153=CARTESIAN_POINT('Ctrl Pts',(10.7915539996106,0.252053558051711,3.4260683625425));
#25154=CARTESIAN_POINT('Ctrl Pts',(10.8074592782982,0.438070873084069,3.55164474938222));
#25155=CARTESIAN_POINT('Ctrl Pts',(10.8233645569858,0.528569890453362,3.72662326908837));
#25156=CARTESIAN_POINT('Ctrl Pts',(10.8392698356734,0.619068907822657,3.90160178879453));
#25157=CARTESIAN_POINT('Ctrl Pts',(10.8551751143611,0.614049627528876,4.12598244136713));
#25158=CARTESIAN_POINT('Ctrl Pts',(10.8710803930487,0.515816690734684,4.29673912390739));
#25159=CARTESIAN_POINT('Ctrl Pts',(10.8869856717363,0.417583753940498,4.46749580644764));
#25160=CARTESIAN_POINT('Ctrl Pts',(10.9028909504239,0.226137160645921,4.58462851895556));
#25161=CARTESIAN_POINT('Ctrl Pts',(10.9187962291115,0.0293810870543861,
4.59435487532392));
#25162=CARTESIAN_POINT('Ctrl Pts',(10.9195823489885,0.0196563998352688,
4.59483560139116));
#25163=CARTESIAN_POINT('Ctrl Pts',(10.9203684688655,0.00991874240631306,
4.5950539509358));
#25164=CARTESIAN_POINT('Ctrl Pts',(10.9211545887425,0.000179316795020235,
4.59501533910171));
#25165=CARTESIAN_POINT('Origin',(4.,0.,4.));
#25166=CARTESIAN_POINT('',(11.3288454112576,-0.000294350894641693,4.59325842069974));
#25167=CARTESIAN_POINT('',(11.2211545887425,0.000456638431143918,4.59352536526061));
#25168=CARTESIAN_POINT('',(4.,-7.27562663373442E-17,4.5941));
#25169=CARTESIAN_POINT('Ctrl Pts',(11.3288454112576,-0.000294350894641693,
4.59325842069974));
#25170=CARTESIAN_POINT('Ctrl Pts',(11.3193914437904,0.117725031793324,4.59273125875086));
#25171=CARTESIAN_POINT('Ctrl Pts',(11.3099374763232,0.236024696118704,4.55868066117597));
#25172=CARTESIAN_POINT('Ctrl Pts',(11.300483508856,0.333060002447629,4.49314500997921));
#25173=CARTESIAN_POINT('Ctrl Pts',(11.2845782301684,0.496311419914153,4.38288835848583));
#25174=CARTESIAN_POINT('Ctrl Pts',(11.2686729514808,0.599375291650127,4.18351506848348));
#25175=CARTESIAN_POINT('Ctrl Pts',(11.2527676727932,0.594929048027223,3.98656891995295));
#25176=CARTESIAN_POINT('Ctrl Pts',(11.2368623941056,0.59048280440432,3.78962277142242));
#25177=CARTESIAN_POINT('Ctrl Pts',(11.220957115418,0.478526445422532,3.5951037643637));
#25178=CARTESIAN_POINT('Ctrl Pts',(11.2050518367303,0.310465594643358,3.49232679739763));
#25179=CARTESIAN_POINT('Ctrl Pts',(11.1891465580427,0.142404743864184,3.38954983043155));
#25180=CARTESIAN_POINT('Ctrl Pts',(11.1732412793551,-0.0817605987123653,
3.37851490355812));
#25181=CARTESIAN_POINT('Ctrl Pts',(11.1573360006675,-0.259103191428711,
3.46428878834836));
#25182=CARTESIAN_POINT('Ctrl Pts',(11.1414307219799,-0.436445784145052,
3.5500626731386));
#25183=CARTESIAN_POINT('Ctrl Pts',(11.1255254432923,-0.566965627001181,
3.73264536959251));
#25184=CARTESIAN_POINT('Ctrl Pts',(11.1096201646047,-0.590733529996744,
3.92820262793532));
#25185=CARTESIAN_POINT('Ctrl Pts',(11.0937148859171,-0.614501432992307,
4.12375988627813));
#25186=CARTESIAN_POINT('Ctrl Pts',(11.0778096072294,-0.531517396127296,
4.33229170650985));
#25187=CARTESIAN_POINT('Ctrl Pts',(11.0619043285418,-0.379884178365051,
4.45804909903384));
#25188=CARTESIAN_POINT('Ctrl Pts',(11.0508846894471,-0.274828280424841,
4.54517747360242));
#25189=CARTESIAN_POINT('Ctrl Pts',(11.0398650503523,-0.136819945681758,
4.59257312212411));
#25190=CARTESIAN_POINT('Ctrl Pts',(11.0288454112576,0.000503618959454472,
4.59367252935801));
#25191=CARTESIAN_POINT('Ctrl Pts',(10.9211545887425,0.000179316795020235,
4.59501533910171));
#25192=CARTESIAN_POINT('Ctrl Pts',(10.9362737475531,-0.187135527734918,
4.59427273168419));
#25193=CARTESIAN_POINT('Ctrl Pts',(10.9513929063637,-0.375104412928531,
4.49848156101044));
#25194=CARTESIAN_POINT('Ctrl Pts',(10.9665120651743,-0.484035620954107,
4.34616539940523));
#25195=CARTESIAN_POINT('Ctrl Pts',(10.982417343862,-0.598630701482551,4.1859295668894));
#25196=CARTESIAN_POINT('Ctrl Pts',(10.9983226225496,-0.625755308650954,
3.96313790162893));
#25197=CARTESIAN_POINT('Ctrl Pts',(11.0142279012372,-0.55295497039508,3.7800869107734));
#25198=CARTESIAN_POINT('Ctrl Pts',(11.0301331799248,-0.480154632139201,
3.59703591991786));
#25199=CARTESIAN_POINT('Ctrl Pts',(11.0460384586124,-0.307429348459053,
3.45372560346725));
#25200=CARTESIAN_POINT('Ctrl Pts',(11.0619437373,-0.114087262216405,3.41595799577618));
#25201=CARTESIAN_POINT('Ctrl Pts',(11.0778490159876,0.0792548240262376,
3.37819038808511));
#25202=CARTESIAN_POINT('Ctrl Pts',(11.0937542946752,0.293213712831377,3.4459654891536));
#25203=CARTESIAN_POINT('Ctrl Pts',(11.1096595733629,0.429548534313776,3.58816383989905));
#25204=CARTESIAN_POINT('Ctrl Pts',(11.1255648520505,0.565883355796175,3.7303621906445));
#25205=CARTESIAN_POINT('Ctrl Pts',(11.1414701307381,0.624594109955846,3.94698379106692));
#25206=CARTESIAN_POINT('Ctrl Pts',(11.1573754094257,0.578723302329844,4.13856516675647));
#25207=CARTESIAN_POINT('Ctrl Pts',(11.1732806881133,0.53285249470384,4.33014654244603));
#25208=CARTESIAN_POINT('Ctrl Pts',(11.1891859668009,0.382400125292158,4.49668769340272));
#25209=CARTESIAN_POINT('Ctrl Pts',(11.2050912454885,0.196447557013804,4.56171996888228));
#25210=CARTESIAN_POINT('Ctrl Pts',(11.2104456932399,0.133847376870746,4.58361282144047));
#25211=CARTESIAN_POINT('Ctrl Pts',(11.2158001409912,0.0672239414478651,
4.5940016224088));
#25212=CARTESIAN_POINT('Ctrl Pts',(11.2211545887425,0.000456638431143918,
4.59352536526061));
#25213=CARTESIAN_POINT('Origin',(4.,0.,4.));
#25214=CARTESIAN_POINT('',(11.6288454112576,-0.000389145320547679,4.59475273347735));
#25215=CARTESIAN_POINT('',(11.5211545887425,-0.0003715675665865,4.59335763259963));
#25216=CARTESIAN_POINT('',(4.,-7.27562663373442E-17,4.5941));
#25217=CARTESIAN_POINT('Ctrl Pts',(11.6288454112576,-0.000389145320547679,
4.59475273347735));
#25218=CARTESIAN_POINT('Ctrl Pts',(11.6148231159161,0.173538999407471,4.59343557735163));
#25219=CARTESIAN_POINT('Ctrl Pts',(11.6008008205746,0.348531733704351,4.51264940831536));
#25220=CARTESIAN_POINT('Ctrl Pts',(11.586778525233,0.459048433726307,4.37867598496766));
#25221=CARTESIAN_POINT('Ctrl Pts',(11.5708732465454,0.584405864209301,4.22671194604376));
#25222=CARTESIAN_POINT('Ctrl Pts',(11.5549679678578,0.626808276394098,4.00631705984067));
#25223=CARTESIAN_POINT('Ctrl Pts',(11.5390626891702,0.566786276503563,3.81868733396413));
#25224=CARTESIAN_POINT('Ctrl Pts',(11.5231574104826,0.506764276613028,3.6310576080876));
#25225=CARTESIAN_POINT('Ctrl Pts',(11.507252131795,0.344317864647159,3.47619304253762));
#25226=CARTESIAN_POINT('Ctrl Pts',(11.4913468531074,0.154035560439752,3.4252008940353));
#25227=CARTESIAN_POINT('Ctrl Pts',(11.4754415744198,-0.0362467437676612,
3.37420874553297));
#25228=CARTESIAN_POINT('Ctrl Pts',(11.4595362957322,-0.254364940216614,
3.4270890140783));
#25229=CARTESIAN_POINT('Ctrl Pts',(11.4436310170445,-0.400168380917644,
3.55956131753494));
#25230=CARTESIAN_POINT('Ctrl Pts',(11.4277257383569,-0.545971821618673,
3.69203362099157));
#25231=CARTESIAN_POINT('Ctrl Pts',(11.4118204596693,-0.619460506571779,
3.90409795935952));
#25232=CARTESIAN_POINT('Ctrl Pts',(11.3959151809817,-0.586891540696359,
4.09838336016249));
#25233=CARTESIAN_POINT('Ctrl Pts',(11.3800099022941,-0.554322574820941,
4.29266876096545));
#25234=CARTESIAN_POINT('Ctrl Pts',(11.3641046236065,-0.415695958117004,
4.46917522420345));
#25235=CARTESIAN_POINT('Ctrl Pts',(11.3481993449189,-0.234663168166497,
4.54685844933023));
#25236=CARTESIAN_POINT('Ctrl Pts',(11.3417480336984,-0.161234786808821,
4.57836740127901));
#25237=CARTESIAN_POINT('Ctrl Pts',(11.335296722478,-0.080829826651965,4.59361815176584));
#25238=CARTESIAN_POINT('Ctrl Pts',(11.3288454112576,-0.000294350894641693,
4.59325842069974));
#25239=CARTESIAN_POINT('Ctrl Pts',(11.2211545887425,0.000456638431143918,
4.59352536526061));
#25240=CARTESIAN_POINT('Ctrl Pts',(11.2317054196788,-0.131106980996848,
4.59258691018808));
#25241=CARTESIAN_POINT('Ctrl Pts',(11.2422562506151,-0.263229208150973,
4.54946171071576));
#25242=CARTESIAN_POINT('Ctrl Pts',(11.2528070815514,-0.366229002642205,
4.4690386804108));
#25243=CARTESIAN_POINT('Ctrl Pts',(11.268712360239,-0.521500226874852,4.34780171645731));
#25244=CARTESIAN_POINT('Ctrl Pts',(11.2846176389266,-0.610589908195122,
4.1418043885479));
#25245=CARTESIAN_POINT('Ctrl Pts',(11.3005229176142,-0.592591834014348,
3.94563195463032));
#25246=CARTESIAN_POINT('Ctrl Pts',(11.3164281963018,-0.574593759833574,
3.74945952071274));
#25247=CARTESIAN_POINT('Ctrl Pts',(11.3323334749894,-0.449507930151742,
3.56311198078699));
#25248=CARTESIAN_POINT('Ctrl Pts',(11.3482387536771,-0.274768466013715,
3.47215224147272));
#25249=CARTESIAN_POINT('Ctrl Pts',(11.3641440323647,-0.100029001875688,
3.38119250215845));
#25250=CARTESIAN_POINT('Ctrl Pts',(11.3800493110523,0.12436409671854,3.38562056345565));
#25251=CARTESIAN_POINT('Ctrl Pts',(11.3959545897399,0.295379012183608,3.48340324695247));
#25252=CARTESIAN_POINT('Ctrl Pts',(11.4118598684275,0.466393927648671,3.5811859304493));
#25253=CARTESIAN_POINT('Ctrl Pts',(11.4277651471151,0.584030659984583,3.77232323614575));
#25254=CARTESIAN_POINT('Ctrl Pts',(11.4436704258027,0.594275398502411,3.96905299961855));
#25255=CARTESIAN_POINT('Ctrl Pts',(11.4595757044903,0.60452013702024,4.16578276309136));
#25256=CARTESIAN_POINT('Ctrl Pts',(11.475480983178,0.507372881719984,4.36810498434052));
#25257=CARTESIAN_POINT('Ctrl Pts',(11.4913862618656,0.34743954227408,4.48312185891572));
#25258=CARTESIAN_POINT('Ctrl Pts',(11.5013090374912,0.247662438486696,4.55487707062799));
#25259=CARTESIAN_POINT('Ctrl Pts',(11.5112318131169,0.123448374926332,4.59265218509947));
#25260=CARTESIAN_POINT('Ctrl Pts',(11.5211545887425,-0.0003715675665865,
4.59335763259963));
#25261=CARTESIAN_POINT('Origin',(4.,0.,4.));
#25262=CARTESIAN_POINT('',(11.9288454112576,0.000492284285450728,4.5944814532616));
#25263=CARTESIAN_POINT('',(11.8211545887425,-0.000307672146732893,4.59488449882539));
#25264=CARTESIAN_POINT('',(4.,-7.27562663373442E-17,4.5941));
#25265=CARTESIAN_POINT('Ctrl Pts',(11.9288454112576,0.000492284285450728,
4.5944814532616));
#25266=CARTESIAN_POINT('Ctrl Pts',(11.9261600667293,0.0338400408399785,
4.59477876231094));
#25267=CARTESIAN_POINT('Ctrl Pts',(11.9234747222011,0.0671420792079604,
4.59221542322669));
#25268=CARTESIAN_POINT('Ctrl Pts',(11.9207893776729,0.0999293694653808,
4.5866302815369));
#25269=CARTESIAN_POINT('Ctrl Pts',(11.9048840989853,0.294128282668868,4.55354952256816));
#25270=CARTESIAN_POINT('Ctrl Pts',(11.8889788202977,0.470268877700486,4.41445832512751));
#25271=CARTESIAN_POINT('Ctrl Pts',(11.8730735416101,0.547474845215755,4.2332214826164));
#25272=CARTESIAN_POINT('Ctrl Pts',(11.8571682629225,0.624680812731027,4.05198464010529));
#25273=CARTESIAN_POINT('Ctrl Pts',(11.8412629842349,0.602952152729945,3.82860215252373));
#25274=CARTESIAN_POINT('Ctrl Pts',(11.8253577055472,0.492265746621211,3.66564180763548));
#25275=CARTESIAN_POINT('Ctrl Pts',(11.8094524268596,0.38157934051248,3.50268146274723));
#25276=CARTESIAN_POINT('Ctrl Pts',(11.793547148172,0.181935188296101,3.40014326055229));
#25277=CARTESIAN_POINT('Ctrl Pts',(11.7776418694844,-0.0149985615777061,
3.40510840546499));
#25278=CARTESIAN_POINT('Ctrl Pts',(11.7617365907968,-0.211932311451519,
3.41007355037768));
#25279=CARTESIAN_POINT('Ctrl Pts',(11.7458313121092,-0.406155658982761,
3.52254204239802));
#25280=CARTESIAN_POINT('Ctrl Pts',(11.7299260334216,-0.508489459897291,
3.69087310813977));
#25281=CARTESIAN_POINT('Ctrl Pts',(11.714020754734,-0.610823260811815,3.8592041738815));
#25282=CARTESIAN_POINT('Ctrl Pts',(11.6981154760463,-0.621267515109637,
4.08339781334463));
#25283=CARTESIAN_POINT('Ctrl Pts',(11.6822101973587,-0.53502666307716,4.26051379213839));
#25284=CARTESIAN_POINT('Ctrl Pts',(11.6663049186711,-0.448785811044678,
4.43762977093217));
#25285=CARTESIAN_POINT('Ctrl Pts',(11.6503996399835,-0.265859852681883,
4.56766808905658));
#25286=CARTESIAN_POINT('Ctrl Pts',(11.6344943612959,-0.070240649109886,
4.59092065229643));
#25287=CARTESIAN_POINT('Ctrl Pts',(11.6326113779498,-0.0470818155087989,
4.59367346098309));
#25288=CARTESIAN_POINT('Ctrl Pts',(11.6307283946037,-0.0237450789937817,
4.59492960773286));
#25289=CARTESIAN_POINT('Ctrl Pts',(11.6288454112576,-0.000389145320547679,
4.59475273347735));
#25290=CARTESIAN_POINT('Ctrl Pts',(11.5211545887425,-0.0003715675665865,
4.59335763259963));
#25291=CARTESIAN_POINT('Ctrl Pts',(11.5271370918045,-0.0750233800274846,
4.5937829512795));
#25292=CARTESIAN_POINT('Ctrl Pts',(11.5331195948664,-0.149531931096223,
4.58073359799715));
#25293=CARTESIAN_POINT('Ctrl Pts',(11.5391020979284,-0.218455391669058,
4.55353248138526));
#25294=CARTESIAN_POINT('Ctrl Pts',(11.555007376616,-0.40169756257477,4.48121470137836));
#25295=CARTESIAN_POINT('Ctrl Pts',(11.5709126553036,-0.545462480794654,
4.3088676134633));
#25296=CARTESIAN_POINT('Ctrl Pts',(11.5868179339912,-0.583739378074245,
4.1156257090067));
#25297=CARTESIAN_POINT('Ctrl Pts',(11.6027232126789,-0.622016275353834,
3.92238380455011));
#25298=CARTESIAN_POINT('Ctrl Pts',(11.6186284913665,-0.554805151693135,
3.70824708355197));
#25299=CARTESIAN_POINT('Ctrl Pts',(11.6345337700541,-0.412966511608993,
3.57153806891708));
#25300=CARTESIAN_POINT('Ctrl Pts',(11.6504390487417,-0.271127871524847,
3.43482905428217));
#25301=CARTESIAN_POINT('Ctrl Pts',(11.6663443274293,-0.0546617150172531,
3.37554774601052));
#25302=CARTESIAN_POINT('Ctrl Pts',(11.6822496061169,0.137039856773353,3.42091361287512));
#25303=CARTESIAN_POINT('Ctrl Pts',(11.6981548848045,0.328741428563947,3.46627947973972));
#25304=CARTESIAN_POINT('Ctrl Pts',(11.7140601634921,0.495678415637556,3.61629252174057));
#25305=CARTESIAN_POINT('Ctrl Pts',(11.7299654421798,0.56120041605148,3.80207309651931));
#25306=CARTESIAN_POINT('Ctrl Pts',(11.7458707208674,0.626722416465409,3.98785367129807));
#25307=CARTESIAN_POINT('Ctrl Pts',(11.761775999555,0.590829430219633,4.20940177885472));
#25308=CARTESIAN_POINT('Ctrl Pts',(11.7776812782426,0.470001998091193,4.36499190112672));
#25309=CARTESIAN_POINT('Ctrl Pts',(11.7921723817426,0.359917612963646,4.5067481450567));
#25310=CARTESIAN_POINT('Ctrl Pts',(11.8066634852425,0.179330777996457,4.59375393408315));
#25311=CARTESIAN_POINT('Ctrl Pts',(11.8211545887425,-0.000307672146732893,
4.59488449882539));
#25312=CARTESIAN_POINT('Origin',(4.,0.,4.));
#25313=CARTESIAN_POINT('',(12.2288454112576,0.000142795628640946,4.59314744373127));
#25314=CARTESIAN_POINT('',(12.1211545887425,0.00052868291625318,4.59430727435519));
#25315=CARTESIAN_POINT('',(4.,-7.27562663373442E-17,4.5941));
#25316=CARTESIAN_POINT('Ctrl Pts',(12.2288454112576,0.000142795628640946,
4.59314744373127));
#25317=CARTESIAN_POINT('Ctrl Pts',(12.221591738855,0.0907369315914116,4.59334157666405));
#25318=CARTESIAN_POINT('Ctrl Pts',(12.2143380664525,0.181251971066953,4.57388161006077));
#25319=CARTESIAN_POINT('Ctrl Pts',(12.2070843940499,0.261922584292681,4.53433840020651));
#25320=CARTESIAN_POINT('Ctrl Pts',(12.1911791153623,0.438810719578057,4.44763117963851));
#25321=CARTESIAN_POINT('Ctrl Pts',(12.1752738366747,0.56836661021043,4.26436322928705));
#25322=CARTESIAN_POINT('Ctrl Pts',(12.1593685579871,0.591103672269137,4.06868343852597));
#25323=CARTESIAN_POINT('Ctrl Pts',(12.1434632792995,0.613840734327844,3.87300364776488));
#25324=CARTESIAN_POINT('Ctrl Pts',(12.1275580006119,0.529758967812885,3.66491201659415));
#25325=CARTESIAN_POINT('Ctrl Pts',(12.1116527219243,0.377465162701742,3.53995541841648));
#25326=CARTESIAN_POINT('Ctrl Pts',(12.0957474432367,0.225171357590603,3.41499882023882));
#25327=CARTESIAN_POINT('Ctrl Pts',(12.0798421645491,0.00466551388328543,
3.37317725505421));
#25328=CARTESIAN_POINT('Ctrl Pts',(12.0639368858614,-0.182805413822737,
3.43369341627091));
#25329=CARTESIAN_POINT('Ctrl Pts',(12.0480316071738,-0.37027634152876,3.49420957748762));
#25330=CARTESIAN_POINT('Ctrl Pts',(12.0321263284862,-0.524712353233489,
3.65706346510565));
#25331=CARTESIAN_POINT('Ctrl Pts',(12.0162210497986,-0.575202966010955,
3.84747946371059));
#25332=CARTESIAN_POINT('Ctrl Pts',(12.000315771111,-0.625693578788423,4.03789546231555));
#25333=CARTESIAN_POINT('Ctrl Pts',(11.9844104924234,-0.572238792638624,
4.25587357190742));
#25334=CARTESIAN_POINT('Ctrl Pts',(11.9685052137358,-0.439382783876041,
4.40132746645495));
#25335=CARTESIAN_POINT('Ctrl Pts',(11.9552852795764,-0.328957325572706,
4.52222386487166));
#25336=CARTESIAN_POINT('Ctrl Pts',(11.942065345417,-0.163678510702966,4.59301780268865));
#25337=CARTESIAN_POINT('Ctrl Pts',(11.9288454112576,0.000492284285450728,
4.5944814532616));
#25338=CARTESIAN_POINT('Ctrl Pts',(11.8211545887425,-0.000307672146732893,
4.59488449882539));
#25339=CARTESIAN_POINT('Ctrl Pts',(11.8225687639301,-0.0178384446610953,
4.59499482973335));
#25340=CARTESIAN_POINT('Ctrl Pts',(11.8239829391178,-0.035360185088601,
4.59428731490513));
#25341=CARTESIAN_POINT('Ctrl Pts',(11.8253971143054,-0.0528064866265509,
4.59273302680715));
#25342=CARTESIAN_POINT('Ctrl Pts',(11.8413023929931,-0.249025661204777,
4.57525189322826));
#25343=CARTESIAN_POINT('Ctrl Pts',(11.8572076716807,-0.435702132350142,
4.45065748908313));
#25344=CARTESIAN_POINT('Ctrl Pts',(11.8731129503683,-0.527121962142897,
4.27615829360067));
#25345=CARTESIAN_POINT('Ctrl Pts',(11.8890182290559,-0.618541791935657,
4.10165909811819));
#25346=CARTESIAN_POINT('Ctrl Pts',(11.9049235077435,-0.614704980375792,
3.87725511129838));
#25347=CARTESIAN_POINT('Ctrl Pts',(11.9208287864311,-0.517373229009482,
3.70598315013913));
#25348=CARTESIAN_POINT('Ctrl Pts',(11.9367340651187,-0.420041477643178,
3.53471118897989));
#25349=CARTESIAN_POINT('Ctrl Pts',(11.9526393438063,-0.229214786470442,
3.41657125348121));
#25350=CARTESIAN_POINT('Ctrl Pts',(11.9685446224939,-0.0325126988662629,
3.4058082039356));
#25351=CARTESIAN_POINT('Ctrl Pts',(11.9844499011816,0.164189388737916,3.39504515438998));
#25352=CARTESIAN_POINT('Ctrl Pts',(12.0003551798692,0.366766872773537,3.49165899079743));
#25353=CARTESIAN_POINT('Ctrl Pts',(12.0162604585568,0.482204742918021,3.65128872687397));
#25354=CARTESIAN_POINT('Ctrl Pts',(12.0321657372444,0.597642613062508,3.81091846295053));
#25355=CARTESIAN_POINT('Ctrl Pts',(12.048071015932,0.625940869315854,4.03356409869619));
#25356=CARTESIAN_POINT('Ctrl Pts',(12.0639762946196,0.554106149607013,4.21699617753661));
#25357=CARTESIAN_POINT('Ctrl Pts',(12.0798815733072,0.482271429898174,4.40042825637702));
#25358=CARTESIAN_POINT('Ctrl Pts',(12.0957868519948,0.310303734227154,4.5446467783122));
#25359=CARTESIAN_POINT('Ctrl Pts',(12.1116921306825,0.117163353092859,4.583432699452));
#25360=CARTESIAN_POINT('Ctrl Pts',(12.1148462833691,0.0788619649798074,
4.59112427906975));
#25361=CARTESIAN_POINT('Ctrl Pts',(12.1180004360558,0.0397279339241207,
4.59466958677844));
#25362=CARTESIAN_POINT('Ctrl Pts',(12.1211545887425,0.00052868291625318,
4.59430727435519));
#25363=CARTESIAN_POINT('Origin',(4.,0.,4.));
#25364=CARTESIAN_POINT('',(12.5288454112576,-0.000545899910317726,4.59395595168017));
#25365=CARTESIAN_POINT('',(12.4211545887425,4.74932194801069E-5,4.59311952367199));
#25366=CARTESIAN_POINT('',(4.,-7.27562663373442E-17,4.5941));
#25367=CARTESIAN_POINT('Ctrl Pts',(12.5288454112576,-0.000545899910317726,
4.59395595168017));
#25368=CARTESIAN_POINT('Ctrl Pts',(12.5170234109807,0.14659828900878,4.5926299020853));
#25369=CARTESIAN_POINT('Ctrl Pts',(12.5052014107038,0.29463204299547,4.53735693360054));
#25370=CARTESIAN_POINT('Ctrl Pts',(12.493379410427,0.402483765871145,4.43832383497591));
#25371=CARTESIAN_POINT('Ctrl Pts',(12.4774741317394,0.547587104485886,4.30508504322883));
#25372=CARTESIAN_POINT('Ctrl Pts',(12.4615688530518,0.619957272242066,4.09263639239171));
#25373=CARTESIAN_POINT('Ctrl Pts',(12.4456635743641,0.586364949835353,3.89852531496775));
#25374=CARTESIAN_POINT('Ctrl Pts',(12.4297582956765,0.55277262742864,3.7044142375438));
#25375=CARTESIAN_POINT('Ctrl Pts',(12.4138530169889,0.41321781485904,3.52864073353302));
#25376=CARTESIAN_POINT('Ctrl Pts',(12.3979477383013,0.231778177981285,3.45191255961345));
#25377=CARTESIAN_POINT('Ctrl Pts',(12.3820424596137,0.0503385411035255,
3.37518438569388));
#25378=CARTESIAN_POINT('Ctrl Pts',(12.3661371809261,-0.172985920082391,
3.39750154186552));
#25379=CARTESIAN_POINT('Ctrl Pts',(12.3502319022385,-0.335654061078685,
3.50861693417539));
#25380=CARTESIAN_POINT('Ctrl Pts',(12.3343266235509,-0.498322202074975,
3.61973232648525));
#25381=CARTESIAN_POINT('Ctrl Pts',(12.3184213448632,-0.600334022881645,
3.81964595493332));
#25382=CARTESIAN_POINT('Ctrl Pts',(12.3025160661756,-0.594850011148503,
4.0165659389844));
#25383=CARTESIAN_POINT('Ctrl Pts',(12.286610787488,-0.58936599941536,4.21348592303547));
#25384=CARTESIAN_POINT('Ctrl Pts',(12.2707055088004,-0.476386155142398,
4.40741226268955));
#25385=CARTESIAN_POINT('Ctrl Pts',(12.2548002301128,-0.307786043036728,
4.50930218712431));
#25386=CARTESIAN_POINT('Ctrl Pts',(12.2461486238277,-0.216076754679914,
4.564724762732));
#25387=CARTESIAN_POINT('Ctrl Pts',(12.2374970175426,-0.107910718865932,
4.59291589733543));
#25388=CARTESIAN_POINT('Ctrl Pts',(12.2288454112576,0.000142795628640946,
4.59314744373127));
#25389=CARTESIAN_POINT('Ctrl Pts',(12.1211545887425,0.00052868291625318,
4.59430727435519));
#25390=CARTESIAN_POINT('Ctrl Pts',(12.1339057147434,-0.157940052872902,
4.59284257311225));
#25391=CARTESIAN_POINT('Ctrl Pts',(12.1466568407444,-0.317474678016714,
4.52751565545538));
#25392=CARTESIAN_POINT('Ctrl Pts',(12.1594079667453,-0.427372353356377,
4.41409399619463));
#25393=CARTESIAN_POINT('Ctrl Pts',(12.1753132454329,-0.564454612073754,
4.27261605145303));
#25394=CARTESIAN_POINT('Ctrl Pts',(12.1912185241205,-0.62430606291093,4.0563068416254));
#25395=CARTESIAN_POINT('Ctrl Pts',(12.2071238028081,-0.579445451749542,
3.8644864045766));
#25396=CARTESIAN_POINT('Ctrl Pts',(12.2230290814957,-0.534584840588155,
3.6726659675278));
#25397=CARTESIAN_POINT('Ctrl Pts',(12.2389343601834,-0.38501216742821,3.50533430325784));
#25398=CARTESIAN_POINT('Ctrl Pts',(12.254839638871,-0.199404875886796,3.43932303278057));
#25399=CARTESIAN_POINT('Ctrl Pts',(12.2707449175586,-0.0137975843453769,
3.37331176230329));
#25400=CARTESIAN_POINT('Ctrl Pts',(12.2866501962462,0.207844325577514,3.40862088561871));
#25401=CARTESIAN_POINT('Ctrl Pts',(12.3025554749338,0.363752265741203,3.52903794710619));
#25402=CARTESIAN_POINT('Ctrl Pts',(12.3184607536214,0.519660205904889,3.64945500859368));
#25403=CARTESIAN_POINT('Ctrl Pts',(12.334366032309,0.609834176309377,3.85498000825323));
#25404=CARTESIAN_POINT('Ctrl Pts',(12.3502713109967,0.592870104691008,4.05124456128685));
#25405=CARTESIAN_POINT('Ctrl Pts',(12.3661765896843,0.575906033072638,4.24750911432049));
#25406=CARTESIAN_POINT('Ctrl Pts',(12.3820818683719,0.451803919431404,4.4345132207282));
#25407=CARTESIAN_POINT('Ctrl Pts',(12.3979871470595,0.277546204023914,4.52639250633888));
#25408=CARTESIAN_POINT('Ctrl Pts',(12.4057096276205,0.192938958450368,4.57100260157974));
#25409=CARTESIAN_POINT('Ctrl Pts',(12.4134321081815,0.0965080911524262,
4.59318808505049));
#25410=CARTESIAN_POINT('Ctrl Pts',(12.4211545887425,4.74932194801069E-5,
4.59311952367199));
#25411=CARTESIAN_POINT('Origin',(4.,0.,4.));
#25412=CARTESIAN_POINT('',(12.8288454112576,0.000112157221815526,4.59505491513413));
#25413=CARTESIAN_POINT('',(12.7211545887425,-0.000546355209092884,4.59413239245978));
#25414=CARTESIAN_POINT('',(4.,-7.27562663373442E-17,4.5941));
#25415=CARTESIAN_POINT('Ctrl Pts',(12.8288454112576,0.000112157221815526,
4.59505491513413));
#25416=CARTESIAN_POINT('Ctrl Pts',(12.828360361794,0.00612048155630211,
4.59507046002904));
#25417=CARTESIAN_POINT('Ctrl Pts',(12.8278753123304,0.0121283652366354,
4.59498736156652));
#25418=CARTESIAN_POINT('Ctrl Pts',(12.8273902628668,0.0181332013859869,
4.59480429815638));
#25419=CARTESIAN_POINT('Ctrl Pts',(12.8114849841792,0.215038052543873,4.58880145767424));
#25420=CARTESIAN_POINT('Ctrl Pts',(12.7955797054916,0.408666038032992,4.47531104548453));
#25421=CARTESIAN_POINT('Ctrl Pts',(12.779674426804,0.510111378641258,4.30644305748136));
#25422=CARTESIAN_POINT('Ctrl Pts',(12.7637691481164,0.611556719249521,4.1375750694782));
#25423=CARTESIAN_POINT('Ctrl Pts',(12.7478638694288,0.620819414976937,3.9133295056616));
#25424=CARTESIAN_POINT('Ctrl Pts',(12.7319585907412,0.533646427817818,3.7366704418887));
#25425=CARTESIAN_POINT('Ctrl Pts',(12.7160533120536,0.446473440658691,3.56001137811579));
#25426=CARTESIAN_POINT('Ctrl Pts',(12.700148033366,0.26286477061301,3.43093881438659));
#25427=CARTESIAN_POINT('Ctrl Pts',(12.6842427546783,0.0671257511235207,
3.4087174113557));
#25428=CARTESIAN_POINT('Ctrl Pts',(12.6683374759907,-0.128613268365957,
3.38649600832481));
#25429=CARTESIAN_POINT('Ctrl Pts',(12.6524321973031,-0.336482637299241,
3.47112576599221));
#25430=CARTESIAN_POINT('Ctrl Pts',(12.6365269186155,-0.461037535689932,
3.62374828002683));
#25431=CARTESIAN_POINT('Ctrl Pts',(12.6206216399279,-0.585592434080627,
3.77637079406146));
#25432=CARTESIAN_POINT('Ctrl Pts',(12.6047163612403,-0.626832861928724,
3.9969860644633));
#25433=CARTESIAN_POINT('Ctrl Pts',(12.5888110825527,-0.565822959504995,
4.18429689252621));
#25434=CARTESIAN_POINT('Ctrl Pts',(12.5729058038651,-0.504813057081268,
4.37160772058911));
#25435=CARTESIAN_POINT('Ctrl Pts',(12.5570005251774,-0.341552824385721,
4.52561410631309));
#25436=CARTESIAN_POINT('Ctrl Pts',(12.5410952464898,-0.151004453301302,
4.57560283284656));
#25437=CARTESIAN_POINT('Ctrl Pts',(12.5370119680791,-0.102085973774189,
4.58843617527608));
#25438=CARTESIAN_POINT('Ctrl Pts',(12.5329286896683,-0.0513689988622793,
4.59441396466913));
#25439=CARTESIAN_POINT('Ctrl Pts',(12.5288454112576,-0.000545899910317726,
4.59395595168017));
#25440=CARTESIAN_POINT('Ctrl Pts',(12.4211545887425,4.74932194801069E-5,
4.59311952367199));
#25441=CARTESIAN_POINT('Ctrl Pts',(12.4293373868691,-0.102162877376194,
4.59304687552285));
#25442=CARTESIAN_POINT('Ctrl Pts',(12.4375201849957,-0.204406628577491,
4.5679880979308));
#25443=CARTESIAN_POINT('Ctrl Pts',(12.4457029831223,-0.292652646395614,
4.51814611323009));
#25444=CARTESIAN_POINT('Ctrl Pts',(12.4616082618099,-0.46418046423393,4.42126596969699));
#25445=CARTESIAN_POINT('Ctrl Pts',(12.4775135404976,-0.582822782736806,
4.23075121781716));
#25446=CARTESIAN_POINT('Ctrl Pts',(12.4934188191852,-0.594104068590283,
4.03407817163935));
#25447=CARTESIAN_POINT('Ctrl Pts',(12.5093240978728,-0.605385354443759,
3.83740512546155));
#25448=CARTESIAN_POINT('Ctrl Pts',(12.5252293765604,-0.509305607647849,
3.63457378498577));
#25449=CARTESIAN_POINT('Ctrl Pts',(12.541134655248,-0.34998058313236,3.51871572067214));
#25450=CARTESIAN_POINT('Ctrl Pts',(12.5570399339356,-0.19065555861687,3.4028576563585));
#25451=CARTESIAN_POINT('Ctrl Pts',(12.5729452126232,0.031914743618199,3.37397286820701));
#25452=CARTESIAN_POINT('Ctrl Pts',(12.5888504913108,0.215535456959467,3.44532402892222));
#25453=CARTESIAN_POINT('Ctrl Pts',(12.6047557699985,0.399156170300736,3.51667518963742));
#25454=CARTESIAN_POINT('Ctrl Pts',(12.6206610486861,0.543827294748204,3.68826229921932));
#25455=CARTESIAN_POINT('Ctrl Pts',(12.6365663273737,0.583121970486127,3.88129981619987));
#25456=CARTESIAN_POINT('Ctrl Pts',(12.6524716060613,0.622416646224052,4.07433733318042));
#25457=CARTESIAN_POINT('Ctrl Pts',(12.6683768847489,0.556334873252426,4.28882525755962));
#25458=CARTESIAN_POINT('Ctrl Pts',(12.6842821634365,0.415218606030559,4.42627980869829));
#25459=CARTESIAN_POINT('Ctrl Pts',(12.6965729718718,0.306170972122536,4.53249785050629));
#25460=CARTESIAN_POINT('Ctrl Pts',(12.7088637803072,0.152317016475741,4.59271595401221));
#25461=CARTESIAN_POINT('Ctrl Pts',(12.7211545887425,-0.000546355209092884,
4.59413239245978));
#25462=CARTESIAN_POINT('Origin',(4.,0.,4.));
#25463=CARTESIAN_POINT('',(13.1288454112576,0.000488576923893258,4.59361798633976));
#25464=CARTESIAN_POINT('',(13.0211545887425,0.000215375668158819,4.59498635240753));
#25465=CARTESIAN_POINT('',(4.,-7.27562663373442E-17,4.5941));
#25466=CARTESIAN_POINT('Ctrl Pts',(13.1288454112576,0.000488576923893258,
4.59361798633976));
#25467=CARTESIAN_POINT('Ctrl Pts',(13.1237920339197,0.0634769139372694,
4.59410397103046));
#25468=CARTESIAN_POINT('Ctrl Pts',(13.1187386565818,0.126326538027094,4.58487602541266));
#25469=CARTESIAN_POINT('Ctrl Pts',(13.1136852792439,0.185787091792062,4.56533540718874));
#25470=CARTESIAN_POINT('Ctrl Pts',(13.0977800005563,0.372936519850693,4.50383218710482));
#25471=CARTESIAN_POINT('Ctrl Pts',(13.0818747218686,0.526512210440984,4.34016674272733));
#25472=CARTESIAN_POINT('Ctrl Pts',(13.065969443181,0.575998703695535,4.14948732200047));
#25473=CARTESIAN_POINT('Ctrl Pts',(13.0500641644934,0.625485196950086,3.9588079012736));
#25474=CARTESIAN_POINT('Ctrl Pts',(13.0341588858058,0.570882492868891,3.74111450419737));
#25475=CARTESIAN_POINT('Ctrl Pts',(13.0182536071182,0.437261843116128,3.59636272886105));
#25476=CARTESIAN_POINT('Ctrl Pts',(13.0023483284306,0.303641193363369,3.45161095352474));
#25477=CARTESIAN_POINT('Ctrl Pts',(12.986443049743,0.0910025979390456,3.37980079992835));
#25478=CARTESIAN_POINT('Ctrl Pts',(12.9705377710554,-0.10301929613509,3.41390445256627));
#25479=CARTESIAN_POINT('Ctrl Pts',(12.9546324923678,-0.297041190209231,
3.4480081052042));
#25480=CARTESIAN_POINT('Ctrl Pts',(12.9387272136801,-0.472446382933184,
3.58802556407645));
#25481=CARTESIAN_POINT('Ctrl Pts',(12.9228219349925,-0.54869623058984,3.76966673571907));
#25482=CARTESIAN_POINT('Ctrl Pts',(12.9069166563049,-0.624946078246494,
3.95130790736168));
#25483=CARTESIAN_POINT('Ctrl Pts',(12.8910113776173,-0.602040580835857,
4.17457279177466));
#25484=CARTESIAN_POINT('Ctrl Pts',(12.8751060989297,-0.490496973717212,
4.33694759959386));
#25485=CARTESIAN_POINT('Ctrl Pts',(12.8596858697056,-0.382355015061345,
4.49437060399126));
#25486=CARTESIAN_POINT('Ctrl Pts',(12.8442656404816,-0.190898750836606,
4.59456072668396));
#25487=CARTESIAN_POINT('Ctrl Pts',(12.8288454112576,0.000112157221815526,
4.59505491513413));
#25488=CARTESIAN_POINT('Ctrl Pts',(12.7211545887425,-0.000546355209092884,
4.59413239245978));
#25489=CARTESIAN_POINT('Ctrl Pts',(12.7247690589948,-0.0455002825709059,
4.59454893744622));
#25490=CARTESIAN_POINT('Ctrl Pts',(12.7283835292471,-0.0903685417208244,
4.58988016539195));
#25491=CARTESIAN_POINT('Ctrl Pts',(12.7319979994994,-0.13398639330236,4.5798004937111));
#25492=CARTESIAN_POINT('Ctrl Pts',(12.747903278187,-0.325924363941296,4.53544544968711));
#25493=CARTESIAN_POINT('Ctrl Pts',(12.7638085568746,-0.493649543747071,
4.38631418374101));
#25494=CARTESIAN_POINT('Ctrl Pts',(12.7797138355622,-0.560149626020051,
4.20088146397168));
#25495=CARTESIAN_POINT('Ctrl Pts',(12.7956191142498,-0.626649708293032,
4.01544874420235));
#25496=CARTESIAN_POINT('Ctrl Pts',(12.8115243929374,-0.591924693033219,
3.79371457060979));
#25497=CARTESIAN_POINT('Ctrl Pts',(12.827429671625,-0.471918838153678,3.63748989490844));
#25498=CARTESIAN_POINT('Ctrl Pts',(12.8433349503126,-0.351912983274129,
3.48126521920708));
#25499=CARTESIAN_POINT('Ctrl Pts',(12.8592402290002,-0.146626288774854,
3.39055004139693));
#25500=CARTESIAN_POINT('Ctrl Pts',(12.8751455076879,0.0496822801939141,
3.40699693328572));
#25501=CARTESIAN_POINT('Ctrl Pts',(12.8910507863755,0.245990849162665,3.42344382517451));
#25502=CARTESIAN_POINT('Ctrl Pts',(12.9069560650631,0.433321292600904,3.54705278676224));
#25503=CARTESIAN_POINT('Ctrl Pts',(12.9228613437507,0.525659396179275,3.72106781235173));
#25504=CARTESIAN_POINT('Ctrl Pts',(12.9387666224383,0.617997499757654,3.89508283794124));
#25505=CARTESIAN_POINT('Ctrl Pts',(12.9546719011259,0.615343263476151,4.11950392753251));
#25506=CARTESIAN_POINT('Ctrl Pts',(12.9705771798135,0.518915400343756,4.29128641125856));
#25507=CARTESIAN_POINT('Ctrl Pts',(12.9864824585012,0.422487537211366,4.46306889498459));
#25508=CARTESIAN_POINT('Ctrl Pts',(13.0023877371888,0.232286047228094,4.58221277284539));
#25509=CARTESIAN_POINT('Ctrl Pts',(13.0182930158764,0.0356434078328121,
4.59401221668908));
#25510=CARTESIAN_POINT('Ctrl Pts',(13.0192468734984,0.0238505254767134,
4.59471984273368));
#25511=CARTESIAN_POINT('Ctrl Pts',(13.0202007311205,0.0120344772878951,
4.59504140054066));
#25512=CARTESIAN_POINT('Ctrl Pts',(13.0211545887425,0.000215375668158819,
4.59498635240753));
#25513=CARTESIAN_POINT('Origin',(4.,0.,4.));
#25514=CARTESIAN_POINT('',(13.4288454112576,-0.000323145728561625,4.59329116515504));
#25515=CARTESIAN_POINT('',(13.3211545887425,0.000436239896754628,4.59347700091179));
#25516=CARTESIAN_POINT('',(4.,-7.27562663373442E-17,4.5941));
#25517=CARTESIAN_POINT('Ctrl Pts',(13.4288454112576,-0.000323145728561625,
4.59329116515504));
#25518=CARTESIAN_POINT('Ctrl Pts',(13.4192237060453,0.11977362227264,4.59270025156928));
#25519=CARTESIAN_POINT('Ctrl Pts',(13.4096020008331,0.240190260834984,4.55734300206483));
#25520=CARTESIAN_POINT('Ctrl Pts',(13.3999802956209,0.338238798929947,4.48960747645051));
#25521=CARTESIAN_POINT('Ctrl Pts',(13.3840750169333,0.500319146323361,4.37763642888821));
#25522=CARTESIAN_POINT('Ctrl Pts',(13.3681697382457,0.601276083433826,4.17718801339723));
#25523=CARTESIAN_POINT('Ctrl Pts',(13.3522644595581,0.594754455875995,3.9802996620979));
#25524=CARTESIAN_POINT('Ctrl Pts',(13.3363591808704,0.588232828318166,3.78341131079859));
#25525=CARTESIAN_POINT('Ctrl Pts',(13.3204539021828,0.474232636092054,3.59008302369095));
#25526=CARTESIAN_POINT('Ctrl Pts',(13.3045486234952,0.305097944517489,3.48908297116948));
#25527=CARTESIAN_POINT('Ctrl Pts',(13.2886433448076,0.135963252942929,3.388082918648));
#25528=CARTESIAN_POINT('Ctrl Pts',(13.27273806612,-0.0883059379800925,3.3794111007127));
#25529=CARTESIAN_POINT('Ctrl Pts',(13.2568327874324,-0.264734703826722,
3.46704924928509));
#25530=CARTESIAN_POINT('Ctrl Pts',(13.2409275087448,-0.441163469673367,
3.55468739785749));
#25531=CARTESIAN_POINT('Ctrl Pts',(13.2250222300572,-0.569751810443623,
3.7386355129376));
#25532=CARTESIAN_POINT('Ctrl Pts',(13.2091169513696,-0.591457400179852,
3.9344324022836));
#25533=CARTESIAN_POINT('Ctrl Pts',(13.1932116726819,-0.613162989916079,
4.1302292916296));
#25534=CARTESIAN_POINT('Ctrl Pts',(13.1773063939943,-0.527985828618295,
4.33787495524147));
#25535=CARTESIAN_POINT('Ctrl Pts',(13.1614011153067,-0.375035665205916,
4.46202728915223));
#25536=CARTESIAN_POINT('Ctrl Pts',(13.150549213957,-0.270680367988337,4.54673431669939));
#25537=CARTESIAN_POINT('Ctrl Pts',(13.1396973126073,-0.134776053786733,
4.59257435599745));
#25538=CARTESIAN_POINT('Ctrl Pts',(13.1288454112576,0.000488576923893258,
4.59361798633976));
#25539=CARTESIAN_POINT('Ctrl Pts',(13.0211545887425,0.000215375668158819,
4.59498635240753));
#25540=CARTESIAN_POINT('Ctrl Pts',(13.0361060098081,-0.185045360160338,
4.59412349007018));
#25541=CARTESIAN_POINT('Ctrl Pts',(13.0510574308736,-0.371056311319581,
4.5007301079696));
#25542=CARTESIAN_POINT('Ctrl Pts',(13.0660088519392,-0.480360474535337,
4.35124746348123));
#25543=CARTESIAN_POINT('Ctrl Pts',(13.0819141306268,-0.596637928700896,
4.19222825660313));
#25544=CARTESIAN_POINT('Ctrl Pts',(13.0978194093145,-0.626109048224722,
3.96973483302036));
#25545=CARTESIAN_POINT('Ctrl Pts',(13.1137246880021,-0.555241941841719,
3.78592675992164));
#25546=CARTESIAN_POINT('Ctrl Pts',(13.1296299666897,-0.484374835458714,
3.60211868682292));
#25547=CARTESIAN_POINT('Ctrl Pts',(13.1455352453773,-0.313169503168878,
3.45699596420825));
#25548=CARTESIAN_POINT('Ctrl Pts',(13.1614405240649,-0.120236190459409,
3.4171928066662));
#25549=CARTESIAN_POINT('Ctrl Pts',(13.1773458027525,0.0726971222500488,
3.37738964912416));
#25550=CARTESIAN_POINT('Ctrl Pts',(13.1932510814401,0.287358415379145,3.44290605665475));
#25551=CARTESIAN_POINT('Ctrl Pts',(13.2091563601277,0.425184304693362,3.58365966669054));
#25552=CARTESIAN_POINT('Ctrl Pts',(13.2250616388154,0.563010194007583,3.72441327672633));
#25553=CARTESIAN_POINT('Ctrl Pts',(13.240966917503,0.624000679506934,3.94040408926733));
#25554=CARTESIAN_POINT('Ctrl Pts',(13.2568721961906,0.580151510544767,4.13245826101242));
#25555=CARTESIAN_POINT('Ctrl Pts',(13.2727774748782,0.536302341582597,4.32451243275751));
#25556=CARTESIAN_POINT('Ctrl Pts',(13.2886827535658,0.387613518158899,4.49262996370669));
#25557=CARTESIAN_POINT('Ctrl Pts',(13.3045880322534,0.202356657484476,4.55961839611428));
#25558=CARTESIAN_POINT('Ctrl Pts',(13.3101102177498,0.13803695776657,4.58287624384712));
#25559=CARTESIAN_POINT('Ctrl Pts',(13.3156324032461,0.0693092633201986,
4.59394375907155));
#25560=CARTESIAN_POINT('Ctrl Pts',(13.3211545887425,0.000436239896754628,
4.59347700091179));
#25561=CARTESIAN_POINT('Origin',(4.,0.,4.));
#25562=CARTESIAN_POINT('',(13.7288454112576,-0.000361622974213827,4.59480268714608));
#25563=CARTESIAN_POINT('',(13.6211545887425,-0.000396530615921017,4.59339874939382));
#25564=CARTESIAN_POINT('',(4.,-7.27562663373442E-17,4.5941));
#25565=CARTESIAN_POINT('Ctrl Pts',(13.7288454112576,-0.000361622974213827,
4.59480268714608));
#25566=CARTESIAN_POINT('Ctrl Pts',(13.714655378171,0.175608319374377,4.59354294412002));
#25567=CARTESIAN_POINT('Ctrl Pts',(13.7004653450845,0.352610168065205,4.51056419690263));
#25568=CARTESIAN_POINT('Ctrl Pts',(13.6862753119979,0.463013835099274,4.37381700684221));
#25569=CARTESIAN_POINT('Ctrl Pts',(13.6703700333103,0.586762742631886,4.22054025587244));
#25570=CARTESIAN_POINT('Ctrl Pts',(13.6544647546227,0.626840040937572,3.99971072753873));
#25571=CARTESIAN_POINT('Ctrl Pts',(13.6385594759351,0.564843930165024,3.81272399872504));
#25572=CARTESIAN_POINT('Ctrl Pts',(13.6226541972475,0.502847819392478,3.62573726991136));
#25573=CARTESIAN_POINT('Ctrl Pts',(13.6067489185599,0.338778299541704,3.4725933406177));
#25574=CARTESIAN_POINT('Ctrl Pts',(13.5908436398723,0.147969152919217,3.42360942419035));
#25575=CARTESIAN_POINT('Ctrl Pts',(13.5749383611846,-0.0428399937032757,
3.37462550776301));
#25576=CARTESIAN_POINT('Ctrl Pts',(13.559033082497,-0.260388767097474,3.42980160420198));
#25577=CARTESIAN_POINT('Ctrl Pts',(13.5431278038094,-0.404787974250376,
3.56380318433064));
#25578=CARTESIAN_POINT('Ctrl Pts',(13.5272225251218,-0.549187181403275,
3.6978047644593));
#25579=CARTESIAN_POINT('Ctrl Pts',(13.5113172464342,-0.620436822314871,
3.91063182827765));
#25580=CARTESIAN_POINT('Ctrl Pts',(13.4954119677466,-0.585822076202281,
4.10456319205082));
#25581=CARTESIAN_POINT('Ctrl Pts',(13.479506689059,-0.551207330089691,4.298494555824));
#25582=CARTESIAN_POINT('Ctrl Pts',(13.4636014103714,-0.410728196952908,
4.47353021955202));
#25583=CARTESIAN_POINT('Ctrl Pts',(13.4476961316837,-0.228886751546343,
4.54930121159921));
#25584=CARTESIAN_POINT('Ctrl Pts',(13.4414125582084,-0.15704808052867,4.57923546205676));
#25585=CARTESIAN_POINT('Ctrl Pts',(13.435128984733,-0.0787538239969463,
4.5936770685736));
#25586=CARTESIAN_POINT('Ctrl Pts',(13.4288454112576,-0.000323145728561625,
4.59329116515504));
#25587=CARTESIAN_POINT('Ctrl Pts',(13.3211545887425,0.000436239896754628,
4.59347700091179));
#25588=CARTESIAN_POINT('Ctrl Pts',(13.3315376819337,-0.129062311182503,
4.59259937855127));
#25589=CARTESIAN_POINT('Ctrl Pts',(13.341920775125,-0.259074650003773,4.55094414667863));
#25590=CARTESIAN_POINT('Ctrl Pts',(13.3523038683163,-0.361265427801182,
4.47287234722855));
#25591=CARTESIAN_POINT('Ctrl Pts',(13.3682091470039,-0.517805754487323,
4.35327853206923));
#25592=CARTESIAN_POINT('Ctrl Pts',(13.3841144256915,-0.609061509934468,
4.14823156788458));
#25593=CARTESIAN_POINT('Ctrl Pts',(13.4000197043791,-0.593131911953917,
3.95188034580653));
#25594=CARTESIAN_POINT('Ctrl Pts',(13.4159249830667,-0.577202313973367,
3.75552912372848));
#25595=CARTESIAN_POINT('Ctrl Pts',(13.4318302617543,-0.454087362565127,
3.56787364375704));
#25596=CARTESIAN_POINT('Ctrl Pts',(13.4477355404419,-0.280316234851803,
3.47507736324643));
#25597=CARTESIAN_POINT('Ctrl Pts',(13.4636408191295,-0.106545107138479,
3.38228108273583));
#25598=CARTESIAN_POINT('Ctrl Pts',(13.4795460978172,0.117882196879929,3.38434400168606));
#25599=CARTESIAN_POINT('Ctrl Pts',(13.4954513765048,0.2899181539344,3.48031891499009));
#25600=CARTESIAN_POINT('Ctrl Pts',(13.5113566551924,0.461954110988876,3.57629382829412));
#25601=CARTESIAN_POINT('Ctrl Pts',(13.52726193388,0.581598721079409,3.76618073595195));
#25602=CARTESIAN_POINT('Ctrl Pts',(13.5431672125676,0.593916240998451,3.96279160341967));
#25603=CARTESIAN_POINT('Ctrl Pts',(13.5590724912552,0.606233760917493,4.15940247088739));
#25604=CARTESIAN_POINT('Ctrl Pts',(13.5749777699428,0.511224190665043,4.362737298165));
#25605=CARTESIAN_POINT('Ctrl Pts',(13.5908830486304,0.352511905377589,4.47943333495374));
#25606=CARTESIAN_POINT('Ctrl Pts',(13.6009735620011,0.251822790258117,4.55346680161908));
#25607=CARTESIAN_POINT('Ctrl Pts',(13.6110640753718,0.125494626822297,4.59262991567553));
#25608=CARTESIAN_POINT('Ctrl Pts',(13.6211545887425,-0.000396530615921017,
4.59339874939382));
#25609=CARTESIAN_POINT('Origin',(4.,0.,4.));
#25610=CARTESIAN_POINT('',(14.0288454112576,0.000507412974116619,4.59441995931617));
#25611=CARTESIAN_POINT('',(13.9211545887425,-0.000275297881949146,4.59492513410986));
#25612=CARTESIAN_POINT('',(4.,-7.27562663373442E-17,4.5941));
#25613=CARTESIAN_POINT('Ctrl Pts',(14.0288454112576,0.000507412974116619,
4.59441995931617));
#25614=CARTESIAN_POINT('Ctrl Pts',(14.0259923289843,0.0359476882196221,
4.59474138052009));
#25615=CARTESIAN_POINT('Ctrl Pts',(14.0231392467111,0.0713355155074759,
4.59184535342408));
#25616=CARTESIAN_POINT('Ctrl Pts',(14.0202861644378,0.106106362061302,4.58554453803953));
#25617=CARTESIAN_POINT('Ctrl Pts',(14.0043808857502,0.299945849210873,4.55041893875697));
#25618=CARTESIAN_POINT('Ctrl Pts',(13.9884756070626,0.474610768799237,4.40947910659883));
#25619=CARTESIAN_POINT('Ctrl Pts',(13.972570328375,0.549902379214768,4.22743864981956));
#25620=CARTESIAN_POINT('Ctrl Pts',(13.9566650496873,0.625193989630293,4.04539819304031));
#25621=CARTESIAN_POINT('Ctrl Pts',(13.9407597709997,0.601112290873006,3.82225711163994));
#25622=CARTESIAN_POINT('Ctrl Pts',(13.9248544923121,0.488714580199595,3.66047234987686));
#25623=CARTESIAN_POINT('Ctrl Pts',(13.9089492136245,0.376316869526181,3.49868758811377));
#25624=CARTESIAN_POINT('Ctrl Pts',(13.8930439349369,0.175603146936639,3.39825914598798));
#25625=CARTESIAN_POINT('Ctrl Pts',(13.8771386562493,-0.0212673376532481,
3.40529951534663));
#25626=CARTESIAN_POINT('Ctrl Pts',(13.8612333775617,-0.218137822243141,
3.41233988470529));
#25627=CARTESIAN_POINT('Ctrl Pts',(13.8453280988741,-0.411165068833379,
3.52684906554841));
#25628=CARTESIAN_POINT('Ctrl Pts',(13.8294228201864,-0.511719132099071,
3.69624928651676));
#25629=CARTESIAN_POINT('Ctrl Pts',(13.8135175414988,-0.612273195364761,
3.8656495074851));
#25630=CARTESIAN_POINT('Ctrl Pts',(13.7976122628112,-0.62035407530591,4.08994076857866));
#25631=CARTESIAN_POINT('Ctrl Pts',(13.7817069841236,-0.532251373727382,
4.26613801168402));
#25632=CARTESIAN_POINT('Ctrl Pts',(13.765801705436,-0.44414867214885,4.44233525478938));
#25633=CARTESIAN_POINT('Ctrl Pts',(13.7498964267484,-0.259862389050636,
4.57043847990653));
#25634=CARTESIAN_POINT('Ctrl Pts',(13.7339911480608,-0.0640089891217576,
4.59162810566218));
#25635=CARTESIAN_POINT('Ctrl Pts',(13.7322759024597,-0.0428879079209441,
4.59391322201126));
#25636=CARTESIAN_POINT('Ctrl Pts',(13.7305606568586,-0.0216323041412813,
4.594954960835));
#25637=CARTESIAN_POINT('Ctrl Pts',(13.7288454112576,-0.000361622974213827,
4.59480268714608));
#25638=CARTESIAN_POINT('Ctrl Pts',(13.6211545887425,-0.000396530615921017,
4.59339874939382));
#25639=CARTESIAN_POINT('Ctrl Pts',(13.6269693540594,-0.0729426448807452,
4.59384179797573));
#25640=CARTESIAN_POINT('Ctrl Pts',(13.6327841193764,-0.145343639818557,
4.58153501668255));
#25641=CARTESIAN_POINT('Ctrl Pts',(13.6385988846933,-0.212609537044371,
4.5558040579697));
#25642=CARTESIAN_POINT('Ctrl Pts',(13.6545041633809,-0.396603693856438,
4.48542149789704));
#25643=CARTESIAN_POINT('Ctrl Pts',(13.6704094420685,-0.542177007158105,
4.31459913145184));
#25644=CARTESIAN_POINT('Ctrl Pts',(13.6863147207561,-0.582488370180261,
4.12177136240739));
#25645=CARTESIAN_POINT('Ctrl Pts',(13.7022199994437,-0.622799733202417,
3.92894359336294));
#25646=CARTESIAN_POINT('Ctrl Pts',(13.7181252781313,-0.557849145945042,
3.71411042171923));
#25647=CARTESIAN_POINT('Ctrl Pts',(13.734030556819,-0.417459170243993,3.57591415105311));
#25648=CARTESIAN_POINT('Ctrl Pts',(13.7499358355066,-0.277069194542941,
3.43771788038699));
#25649=CARTESIAN_POINT('Ctrl Pts',(13.7658411141942,-0.0612398303982075,
3.37615851069845));
#25650=CARTESIAN_POINT('Ctrl Pts',(13.7817463928818,0.130929209162332,3.41950150018632));
#25651=CARTESIAN_POINT('Ctrl Pts',(13.7976516715694,0.323098248722867,3.46284448967418));
#25652=CARTESIAN_POINT('Ctrl Pts',(13.813556950257,0.491606963699209,3.61108983833845));
#25653=CARTESIAN_POINT('Ctrl Pts',(13.8294622289446,0.559083281190044,3.79616955381596));
#25654=CARTESIAN_POINT('Ctrl Pts',(13.8453675076322,0.62655959868088,3.98124926929349));
#25655=CARTESIAN_POINT('Ctrl Pts',(13.8612727863198,0.593003518686204,4.20316335158427));
#25656=CARTESIAN_POINT('Ctrl Pts',(13.8771780650075,0.4738225734989,4.36001824251097));
#25657=CARTESIAN_POINT('Ctrl Pts',(13.8918369062525,0.363981395029584,4.50458099992985));
#25658=CARTESIAN_POINT('Ctrl Pts',(13.9064957474975,0.181409709145346,4.59388191268165));
#25659=CARTESIAN_POINT('Ctrl Pts',(13.9211545887425,-0.000275297881949146,
4.59492513410986));
#25660=CARTESIAN_POINT('Origin',(4.,0.,4.));
#25661=CARTESIAN_POINT('',(14.3288454112576,0.000109044058801022,4.5931342436645));
#25662=CARTESIAN_POINT('',(14.2211545887425,0.000537210645871958,4.59424369460725));
#25663=CARTESIAN_POINT('',(4.,-7.27562663373442E-17,4.5941));
#25664=CARTESIAN_POINT('Ctrl Pts',(14.3288454112576,0.000109044058801022,
4.5931342436645));
#25665=CARTESIAN_POINT('Ctrl Pts',(14.32142400111,0.0928032711674493,4.59328573107644));
#25666=CARTESIAN_POINT('Ctrl Pts',(14.3140025909624,0.185434358886594,4.57287353691408));
#25667=CARTESIAN_POINT('Ctrl Pts',(14.3065811808148,0.267539471941071,4.53154830171049));
#25668=CARTESIAN_POINT('Ctrl Pts',(14.2906759021272,0.443503969097433,4.44298165875801));
#25669=CARTESIAN_POINT('Ctrl Pts',(14.2747706234396,0.571121189235106,4.25835848700565));
#25670=CARTESIAN_POINT('Ctrl Pts',(14.258865344752,0.591794703906212,4.06244993615984));
#25671=CARTESIAN_POINT('Ctrl Pts',(14.2429600660644,0.612468218577319,3.86654138531401));
#25672=CARTESIAN_POINT('Ctrl Pts',(14.2270547873768,0.526198027781844,3.65934745537473));
#25673=CARTESIAN_POINT('Ctrl Pts',(14.2111495086891,0.372595753342289,3.53600283331781));
#25674=CARTESIAN_POINT('Ctrl Pts',(14.1952442300015,0.218993478902743,3.4126582112609));
#25675=CARTESIAN_POINT('Ctrl Pts',(14.1793389513139,-0.00194087918087354,
3.37316289708635));
#25676=CARTESIAN_POINT('Ctrl Pts',(14.1634336726263,-0.18876361063844,3.43565146815417));
#25677=CARTESIAN_POINT('Ctrl Pts',(14.1475283939387,-0.375586342096006,
3.49814003922198));
#25678=CARTESIAN_POINT('Ctrl Pts',(14.1316231152511,-0.528297446927522,
3.66261249553216));
#25679=CARTESIAN_POINT('Ctrl Pts',(14.1157178365635,-0.576778446468407,
3.85355004340287));
#25680=CARTESIAN_POINT('Ctrl Pts',(14.0998125578759,-0.625259446009293,
4.04448759127359));
#25681=CARTESIAN_POINT('Ctrl Pts',(14.0839072791882,-0.569510340259543,
4.26189023070484));
#25682=CARTESIAN_POINT('Ctrl Pts',(14.0680020005006,-0.435128760029281,
4.40593586721696));
#25683=CARTESIAN_POINT('Ctrl Pts',(14.0549498040863,-0.324852491748397,
4.52414265738481));
#25684=CARTESIAN_POINT('Ctrl Pts',(14.0418976076719,-0.161623710204441,
4.5929495310973));
#25685=CARTESIAN_POINT('Ctrl Pts',(14.0288454112576,0.000507412974116619,
4.59441995931617));
#25686=CARTESIAN_POINT('Ctrl Pts',(13.9211545887425,-0.000275297881949146,
4.59492513410986));
#25687=CARTESIAN_POINT('Ctrl Pts',(13.9224010261851,-0.015723926578741,
4.59501383895544));
#25688=CARTESIAN_POINT('Ctrl Pts',(13.9236474636277,-0.0311661445373128,
4.59446443570748));
#25689=CARTESIAN_POINT('Ctrl Pts',(13.9248939010703,-0.0465566941337027,
4.59325663951544));
#25690=CARTESIAN_POINT('Ctrl Pts',(13.9407991797579,-0.242949206199084,
4.5778444460306));
#25691=CARTESIAN_POINT('Ctrl Pts',(13.9567044584455,-0.430928419949921,
4.4552243594983));
#25692=CARTESIAN_POINT('Ctrl Pts',(13.9726097371331,-0.524182233176515,
4.28169833602613));
#25693=CARTESIAN_POINT('Ctrl Pts',(13.9885150158207,-0.617436046403107,
4.10817231255396));
#25694=CARTESIAN_POINT('Ctrl Pts',(14.0044202945084,-0.615964459105464,
3.88374035214192));
#25695=CARTESIAN_POINT('Ctrl Pts',(14.020325573196,-0.52044316191294,3.71145211607799));
#25696=CARTESIAN_POINT('Ctrl Pts',(14.0362308518836,-0.424921864720413,
3.53916388001405));
#25697=CARTESIAN_POINT('Ctrl Pts',(14.0521361305712,-0.235350857633014,
3.41901936829824));
#25698=CARTESIAN_POINT('Ctrl Pts',(14.0680414092588,-0.0387731270173405,
3.40618385781531));
#25699=CARTESIAN_POINT('Ctrl Pts',(14.0839466879464,0.157804603598333,3.39334834733239));
#25700=CARTESIAN_POINT('Ctrl Pts',(14.0998519666341,0.361389057742269,3.48782183808236));
#25701=CARTESIAN_POINT('Ctrl Pts',(14.1157572453217,0.478502867019537,3.64622609995664));
#25702=CARTESIAN_POINT('Ctrl Pts',(14.1316625240093,0.595616676296804,3.80463036183091));
#25703=CARTESIAN_POINT('Ctrl Pts',(14.1475678026969,0.626259840707404,4.02696539482948));
#25704=CARTESIAN_POINT('Ctrl Pts',(14.1634730813845,0.556362315559365,4.21114435801894));
#25705=CARTESIAN_POINT('Ctrl Pts',(14.1793783600721,0.486464790411328,4.3953233212084));
#25706=CARTESIAN_POINT('Ctrl Pts',(14.1952836387597,0.316026575704654,4.54134621458875));
#25707=CARTESIAN_POINT('Ctrl Pts',(14.2111889174473,0.123305688986428,4.58216550323889));
#25708=CARTESIAN_POINT('Ctrl Pts',(14.2145108078791,0.0830550475387342,
4.59069079896363));
#25709=CARTESIAN_POINT('Ctrl Pts',(14.2178326983108,0.0418324306113591,
4.59462708830176));
#25710=CARTESIAN_POINT('Ctrl Pts',(14.2211545887425,0.000537210645871958,
4.59424369460725));
#25711=CARTESIAN_POINT('Origin',(4.,0.,4.));
#25712=CARTESIAN_POINT('',(14.6288454112575,-0.000548182068839831,4.59401855345973));
#25713=CARTESIAN_POINT('',(14.5211545887425,1.28950532977596E-5,4.59311636453746));
#25714=CARTESIAN_POINT('',(4.,-7.27562663373442E-17,4.5941));
#25715=CARTESIAN_POINT('Ctrl Pts',(14.6288454112575,-0.000548182068839831,
4.59401855345973));
#25716=CARTESIAN_POINT('Ctrl Pts',(14.6168556732357,0.148643716013534,4.59265593252186));
#25717=CARTESIAN_POINT('Ctrl Pts',(14.6048659352138,0.29876355451001,4.53564313143304));
#25718=CARTESIAN_POINT('Ctrl Pts',(14.5928761971919,0.407080942069735,4.43405768361063));
#25719=CARTESIAN_POINT('Ctrl Pts',(14.5769709185042,0.55077200793829,4.29929703619113));
#25720=CARTESIAN_POINT('Ctrl Pts',(14.5610656398166,0.620899143473568,4.08609746938767));
#25721=CARTESIAN_POINT('Ctrl Pts',(14.545160361129,0.585262934872208,3.89235120454656));
#25722=CARTESIAN_POINT('Ctrl Pts',(14.5292550824414,0.549626726270847,3.69860493970543));
#25723=CARTESIAN_POINT('Ctrl Pts',(14.5133498037538,0.408227173532835,3.52431197682665));
#25724=CARTESIAN_POINT('Ctrl Pts',(14.4974445250662,0.225988969153725,3.44950027073699));
#25725=CARTESIAN_POINT('Ctrl Pts',(14.4815392463786,0.04375076477463,3.37468856464734));
#25726=CARTESIAN_POINT('Ctrl Pts',(14.465633967691,-0.179326091245555,3.39935811534679));
#25727=CARTESIAN_POINT('Ctrl Pts',(14.4497286890033,-0.340814144225853,
3.51218170883678));
#25728=CARTESIAN_POINT('Ctrl Pts',(14.4338234103157,-0.50230219720616,3.62500530232677));
#25729=CARTESIAN_POINT('Ctrl Pts',(14.4179181316281,-0.602201447146573,
3.82598293860731));
#25730=CARTESIAN_POINT('Ctrl Pts',(14.4020128529405,-0.594642384863179,
4.02283418976097));
#25731=CARTESIAN_POINT('Ctrl Pts',(14.3861075742529,-0.587083322579785,
4.21968544091462));
#25732=CARTESIAN_POINT('Ctrl Pts',(14.3702022955653,-0.47206594807259,4.4124103069414));
#25733=CARTESIAN_POINT('Ctrl Pts',(14.3542970168777,-0.302401373731467,
4.51251768287848));
#25734=CARTESIAN_POINT('Ctrl Pts',(14.3458131483376,-0.211902365642262,
4.565914912441));
#25735=CARTESIAN_POINT('Ctrl Pts',(14.3373292797976,-0.10585540495725,4.59296106912451));
#25736=CARTESIAN_POINT('Ctrl Pts',(14.3288454112576,0.000109044058801022,
4.5931342436645));
#25737=CARTESIAN_POINT('Ctrl Pts',(14.2211545887425,0.000537210645871958,
4.59424369460725));
#25738=CARTESIAN_POINT('Ctrl Pts',(14.2337379769984,-0.155889919212927,
4.59279139152499));
#25739=CARTESIAN_POINT('Ctrl Pts',(14.2463213652543,-0.313358837143528,
4.52935553548989));
#25740=CARTESIAN_POINT('Ctrl Pts',(14.2589047535102,-0.422984449084643,
4.4185751090669));
#25741=CARTESIAN_POINT('Ctrl Pts',(14.2748100321978,-0.561550141707708,
4.27854974232482));
#25742=CARTESIAN_POINT('Ctrl Pts',(14.2907153108854,-0.623677968224056,
4.06288332492072));
#25743=CARTESIAN_POINT('Ctrl Pts',(14.306620589573,-0.580841459108965,3.87060075163287));
#25744=CARTESIAN_POINT('Ctrl Pts',(14.3225258682606,-0.538004949993874,
3.67831817834502));
#25745=CARTESIAN_POINT('Ctrl Pts',(14.3384311469482,-0.390204105247342,
3.50941944917344));
#25746=CARTESIAN_POINT('Ctrl Pts',(14.3543364256359,-0.205302819838896,
3.44145571503774));
#25747=CARTESIAN_POINT('Ctrl Pts',(14.3702417043235,-0.0204015344304391,
3.37349198090203));
#25748=CARTESIAN_POINT('Ctrl Pts',(14.3861469830111,0.201600191639931,3.40646324180223));
#25749=CARTESIAN_POINT('Ctrl Pts',(14.4020522616987,0.358768557879186,3.52523048963197));
#25750=CARTESIAN_POINT('Ctrl Pts',(14.4179575403863,0.515936924118427,3.6439977374617));
#25751=CARTESIAN_POINT('Ctrl Pts',(14.4338628190739,0.608271930526566,3.84856097222098));
#25752=CARTESIAN_POINT('Ctrl Pts',(14.4497680977615,0.59337724853295,4.04499341086509));
#25753=CARTESIAN_POINT('Ctrl Pts',(14.4656733764491,0.578482566539332,4.2414258495092));
#25754=CARTESIAN_POINT('Ctrl Pts',(14.4815786551367,0.456358196143958,4.42972749203816));
#25755=CARTESIAN_POINT('Ctrl Pts',(14.4974839338244,0.283078481576349,4.52343819058819));
#25756=CARTESIAN_POINT('Ctrl Pts',(14.5053741521304,0.197118668938093,4.56992576768087));
#25757=CARTESIAN_POINT('Ctrl Pts',(14.5132643704364,0.0985699939877532,
4.59313537862966));
#25758=CARTESIAN_POINT('Ctrl Pts',(14.5211545887425,1.28950532977596E-5,
4.59311636453746));
#25759=CARTESIAN_POINT('Origin',(4.,0.,4.));
#25760=CARTESIAN_POINT('',(14.9288454112575,0.000149915246051877,4.59503491979621));
#25761=CARTESIAN_POINT('',(14.8211545887425,-0.000542004001680995,4.59419620878869));
#25762=CARTESIAN_POINT('',(4.,-7.27562663373442E-17,4.5941));
#25763=CARTESIAN_POINT('Ctrl Pts',(14.9288454112575,0.000149915246051877,
4.59503491979621));
#25764=CARTESIAN_POINT('Ctrl Pts',(14.9281926240489,0.00823674021970066,
4.59506221957623));
#25765=CARTESIAN_POINT('Ctrl Pts',(14.9275398368403,0.0163225255999611,
4.59491168338633));
#25766=CARTESIAN_POINT('Ctrl Pts',(14.9268870496317,0.0244008833477238,
4.59458015690877));
#25767=CARTESIAN_POINT('Ctrl Pts',(14.9109817709441,0.221231534471853,4.58650245417764));
#25768=CARTESIAN_POINT('Ctrl Pts',(14.8950764922565,0.413652681988333,4.47097768448731));
#25769=CARTESIAN_POINT('Ctrl Pts',(14.8791712135689,0.513312675625014,4.30104993462962));
#25770=CARTESIAN_POINT('Ctrl Pts',(14.8632659348813,0.612972669261697,4.13112218477192));
#25771=CARTESIAN_POINT('Ctrl Pts',(14.8473606561937,0.619871509018575,3.90679145474687));
#25772=CARTESIAN_POINT('Ctrl Pts',(14.831455377506,0.530841539545133,3.73106092513143));
#25773=CARTESIAN_POINT('Ctrl Pts',(14.8155500988184,0.441811570071688,3.55533039551599));
#25774=CARTESIAN_POINT('Ctrl Pts',(14.7996448201308,0.256852791367914,3.42820006631018));
#25775=CARTESIAN_POINT('Ctrl Pts',(14.7837395414432,0.0608904496539635,
3.40804280624462));
#25776=CARTESIAN_POINT('Ctrl Pts',(14.7678342627556,-0.135071892059981,
3.38788554617906));
#25777=CARTESIAN_POINT('Ctrl Pts',(14.751928984068,-0.342037796784102,3.47470135525375));
#25778=CARTESIAN_POINT('Ctrl Pts',(14.7360237053804,-0.464977277074429,
3.62862808681558));
#25779=CARTESIAN_POINT('Ctrl Pts',(14.7201184266927,-0.587916757364756,
3.78255481837741));
#25780=CARTESIAN_POINT('Ctrl Pts',(14.7042131480052,-0.62682981322129,4.00359247242638));
#25781=CARTESIAN_POINT('Ctrl Pts',(14.6883078693175,-0.56384921567034,4.19024990955517));
#25782=CARTESIAN_POINT('Ctrl Pts',(14.6724025906299,-0.500868618119389,
4.37690734668397));
#25783=CARTESIAN_POINT('Ctrl Pts',(14.6564973119423,-0.335994367160947,
4.52918456689258));
#25784=CARTESIAN_POINT('Ctrl Pts',(14.6405920332547,-0.144929743580805,
4.57716231297912));
#25785=CARTESIAN_POINT('Ctrl Pts',(14.636676492589,-0.097893704910838,4.5889734116427));
#25786=CARTESIAN_POINT('Ctrl Pts',(14.6327609519233,-0.0492704262804658,
4.59446355048005));
#25787=CARTESIAN_POINT('Ctrl Pts',(14.6288454112575,-0.000548182068839831,
4.59401855345973));
#25788=CARTESIAN_POINT('Ctrl Pts',(14.5211545887425,1.28950532977596E-5,
4.59311636453746));
#25789=CARTESIAN_POINT('Ctrl Pts',(14.5291696491241,-0.100103612291989,
4.59309704959697));
#25790=CARTESIAN_POINT('Ctrl Pts',(14.5371847095056,-0.200228812305367,
4.56910822985942));
#25791=CARTESIAN_POINT('Ctrl Pts',(14.5451997698872,-0.287175610734119,
4.52120162576233));
#25792=CARTESIAN_POINT('Ctrl Pts',(14.5611050485748,-0.459714929737158,
4.42613460781534));
#25793=CARTESIAN_POINT('Ctrl Pts',(14.5770103272624,-0.580358509003398,
4.23688081735026));
#25794=CARTESIAN_POINT('Ctrl Pts',(14.59291560595,-0.593711920942704,4.04033758828107));
#25795=CARTESIAN_POINT('Ctrl Pts',(14.6088208846377,-0.607065332882009,
3.84379435921188));
#25796=CARTESIAN_POINT('Ctrl Pts',(14.6247261633253,-0.513128577494387,
3.63996169153858));
#25797=CARTESIAN_POINT('Ctrl Pts',(14.6406314420129,-0.35503343871745,3.52243092280774));
#25798=CARTESIAN_POINT('Ctrl Pts',(14.6565367207005,-0.196938299940509,
3.40490015407689));
#25799=CARTESIAN_POINT('Ctrl Pts',(14.6724419993881,0.025315222225754,3.37367128428849));
#25800=CARTESIAN_POINT('Ctrl Pts',(14.6883472780757,0.209677713173688,3.44308328926485));
#25801=CARTESIAN_POINT('Ctrl Pts',(14.7042525567633,0.394040204121622,3.51249529424121));
#25802=CARTESIAN_POINT('Ctrl Pts',(14.720157835451,0.540511663851219,3.68254817398232));
#25803=CARTESIAN_POINT('Ctrl Pts',(14.7360631141386,0.581838594751101,3.87516084045512));
#25804=CARTESIAN_POINT('Ctrl Pts',(14.7519683928262,0.623165525650983,4.06777350692792));
#25805=CARTESIAN_POINT('Ctrl Pts',(14.7678736715138,0.559347927721136,4.2829459601324));
#25806=CARTESIAN_POINT('Ctrl Pts',(14.7837789502014,0.419688142031033,4.42188011275284));
#25807=CARTESIAN_POINT('Ctrl Pts',(14.7962374963817,0.310293146587505,4.53070672248707));
#25808=CARTESIAN_POINT('Ctrl Pts',(14.8086960425621,0.154364940471616,4.59275708529138));
#25809=CARTESIAN_POINT('Ctrl Pts',(14.8211545887425,-0.000542004001680995,
4.59419620878869));
#25810=CARTESIAN_POINT('Origin',(4.,0.,4.));
#25811=CARTESIAN_POINT('',(15.2288454112576,0.000471544078774977,4.59356550157774));
#25812=CARTESIAN_POINT('',(15.1211545887425,0.000250233060073018,4.59495282954609));
#25813=CARTESIAN_POINT('',(4.,-7.27562663373442E-17,4.5941));
#25814=CARTESIAN_POINT('Ctrl Pts',(15.2288454112576,0.000471544078774977,
4.59356550157774));
#25815=CARTESIAN_POINT('Ctrl Pts',(15.2236242961746,0.0655651715058866,
4.59404721416646));
#25816=CARTESIAN_POINT('Ctrl Pts',(15.2184031810917,0.130516835945995,4.58418155789741));
#25817=CARTESIAN_POINT('Ctrl Pts',(15.2131820660088,0.191734887706884,4.56334598510492));
#25818=CARTESIAN_POINT('Ctrl Pts',(15.1972767873211,0.378225734681762,4.49987379829874));
#25819=CARTESIAN_POINT('Ctrl Pts',(15.1813715086335,0.530068013118856,4.33459889729257));
#25820=CARTESIAN_POINT('Ctrl Pts',(15.1654662299459,0.577542172676889,4.143408524424));
#25821=CARTESIAN_POINT('Ctrl Pts',(15.1495609512583,0.625016332234921,3.95221815155542));
#25822=CARTESIAN_POINT('Ctrl Pts',(15.1336556725707,0.568122372913892,3.73511230682445));
#25823=CARTESIAN_POINT('Ctrl Pts',(15.1177503938831,0.432983593849097,3.59177680914072));
#25824=CARTESIAN_POINT('Ctrl Pts',(15.1018451151955,0.297844814784303,3.44844131145699));
#25825=CARTESIAN_POINT('Ctrl Pts',(15.0859398365078,0.0844612159757424,
3.37887616082051));
#25826=CARTESIAN_POINT('Ctrl Pts',(15.0700345578202,-0.109190481519281,
3.41502273134472));
#25827=CARTESIAN_POINT('Ctrl Pts',(15.0541292791326,-0.302842179014298,
3.45116930186893));
#25828=CARTESIAN_POINT('Ctrl Pts',(15.038224000445,-0.47676197519578,3.59302759355383));
#25829=CARTESIAN_POINT('Ctrl Pts',(15.0223187217574,-0.551093257596978,
3.77546228038711));
#25830=CARTESIAN_POINT('Ctrl Pts',(15.0064134430698,-0.625424539998176,
3.95789696722038));
#25831=CARTESIAN_POINT('Ctrl Pts',(14.9905081643822,-0.600167308619091,
4.18090804920204));
#25832=CARTESIAN_POINT('Ctrl Pts',(14.9746028856946,-0.486918615563658,
4.34209827230691));
#25833=CARTESIAN_POINT('Ctrl Pts',(14.9593503942156,-0.378317895025423,
4.49667289829699));
#25834=CARTESIAN_POINT('Ctrl Pts',(14.9440979027365,-0.188800216398263,
4.59439705548643));
#25835=CARTESIAN_POINT('Ctrl Pts',(14.9288454112575,0.000149915246051877,
4.59503491979621));
#25836=CARTESIAN_POINT('Ctrl Pts',(14.8211545887425,-0.000542004001680995,
4.59419620878869));
#25837=CARTESIAN_POINT('Ctrl Pts',(14.8246013212497,-0.0433979515083632,
4.5945943510493));
#25838=CARTESIAN_POINT('Ctrl Pts',(14.828048053757,-0.0861757330942537,
4.59035339483295));
#25839=CARTESIAN_POINT('Ctrl Pts',(14.8314947862642,-0.127868389248254,
4.58118038604969));
#25840=CARTESIAN_POINT('Ctrl Pts',(14.8474000649518,-0.320263161387096,
4.5388506546897));
#25841=CARTESIAN_POINT('Ctrl Pts',(14.8633053436395,-0.489550732214419,
4.39149533993331));
#25842=CARTESIAN_POINT('Ctrl Pts',(14.8792106223271,-0.558001411172811,
4.20677376822741));
#25843=CARTESIAN_POINT('Ctrl Pts',(14.8951159010147,-0.6264520901312,4.0220521965215));
#25844=CARTESIAN_POINT('Ctrl Pts',(14.9110211797023,-0.594065877220663,
3.79996436786608));
#25845=CARTESIAN_POINT('Ctrl Pts',(14.9269264583899,-0.475713151262041,
3.64248361741852));
#25846=CARTESIAN_POINT('Ctrl Pts',(14.9428317370775,-0.357360425303418,
3.48500286697096));
#25847=CARTESIAN_POINT('Ctrl Pts',(14.9587370157651,-0.153041186296697,
3.39212919473125));
#25848=CARTESIAN_POINT('Ctrl Pts',(14.9746422944528,0.0434298152403689,
3.40650626183085));
#25849=CARTESIAN_POINT('Ctrl Pts',(14.9905475731404,0.239900816777435,3.42088332893044));
#25850=CARTESIAN_POINT('Ctrl Pts',(15.006452851828,0.428523580844854,3.54251113536931));
#25851=CARTESIAN_POINT('Ctrl Pts',(15.0223581305156,0.522690514153935,3.71554333807889));
#25852=CARTESIAN_POINT('Ctrl Pts',(15.0382634092032,0.616857447463019,3.88857554078846));
#25853=CARTESIAN_POINT('Ctrl Pts',(15.0541686878908,0.616568550013756,4.11301213976874));
#25854=CARTESIAN_POINT('Ctrl Pts',(15.0700739665784,0.521956471292605,4.28580134389743));
#25855=CARTESIAN_POINT('Ctrl Pts',(15.085979245266,0.427344392571456,4.45859054802613));
#25856=CARTESIAN_POINT('Ctrl Pts',(15.1018845239536,0.238409132578427,4.57973235730324));
#25857=CARTESIAN_POINT('Ctrl Pts',(15.1177898026413,0.0419017695106382,
4.59360357799603));
#25858=CARTESIAN_POINT('Ctrl Pts',(15.1189113980083,0.0280446248267054,
4.59458173733358));
#25859=CARTESIAN_POINT('Ctrl Pts',(15.1200329933754,0.0141498265549413,
4.59502647517791));
#25860=CARTESIAN_POINT('Ctrl Pts',(15.1211545887425,0.000250233060073018,
4.59495282954609));
#25861=CARTESIAN_POINT('Origin',(4.,0.,4.));
#25862=CARTESIAN_POINT('',(15.5288454112575,-0.000350670266729247,4.59332700645389));
#25863=CARTESIAN_POINT('',(15.4211545887425,0.000414092275955974,4.59343115273787));
#25864=CARTESIAN_POINT('',(4.,-7.27562663373442E-17,4.5941));
#25865=CARTESIAN_POINT('Ctrl Pts',(15.5288454112575,-0.000350670266729247,
4.59332700645389));
#25866=CARTESIAN_POINT('Ctrl Pts',(15.5190559683003,0.121821298278883,4.59267222728074));
#25867=CARTESIAN_POINT('Ctrl Pts',(15.509266525343,0.244354036528086,4.55597946496206));
#25868=CARTESIAN_POINT('Ctrl Pts',(15.4994770823858,0.343380025451582,4.48601555964668));
#25869=CARTESIAN_POINT('Ctrl Pts',(15.4835718036982,0.504271299656008,4.37234255322809));
#25870=CARTESIAN_POINT('Ctrl Pts',(15.4676665250105,0.603110088323456,4.17084127710728));
#25871=CARTESIAN_POINT('Ctrl Pts',(15.4517612463229,0.594513801222153,3.97403259246294));
#25872=CARTESIAN_POINT('Ctrl Pts',(15.4358559676353,0.58591751412085,3.7772239078186));
#25873=CARTESIAN_POINT('Ctrl Pts',(15.4199506889477,0.469886151250777,3.58510781465072));
#25874=CARTESIAN_POINT('Ctrl Pts',(15.4040454102601,0.299696405559752,3.48589589518039));
#25875=CARTESIAN_POINT('Ctrl Pts',(15.3881401315725,0.129506659868722,3.38668397571006));
#25876=CARTESIAN_POINT('Ctrl Pts',(15.3722348528849,-0.0948414686432761,
3.38037622993726));
#25877=CARTESIAN_POINT('Ctrl Pts',(15.3563295741973,-0.270336810750117,
3.46986890786216));
#25878=CARTESIAN_POINT('Ctrl Pts',(15.3404242955096,-0.445832152856957,
3.55936158578705));
#25879=CARTESIAN_POINT('Ctrl Pts',(15.324519016822,-0.572474708558633,3.74465468740961));
#25880=CARTESIAN_POINT('Ctrl Pts',(15.3086137381344,-0.592115574081638,
3.94066945956945));
#25881=CARTESIAN_POINT('Ctrl Pts',(15.2927084594468,-0.611756439604643,
4.13668423172929));
#25882=CARTESIAN_POINT('Ctrl Pts',(15.2768031807592,-0.524395614948954,
4.3434206744264));
#25883=CARTESIAN_POINT('Ctrl Pts',(15.2608979020716,-0.370145494864779,
4.46595415947185));
#25884=CARTESIAN_POINT('Ctrl Pts',(15.2502137384669,-0.266529987624151,
4.54826443060822));
#25885=CARTESIAN_POINT('Ctrl Pts',(15.2395295748622,-0.13273198696893,4.59257975504152));
#25886=CARTESIAN_POINT('Ctrl Pts',(15.2288454112576,0.000471544078774977,
4.59356550157774));
#25887=CARTESIAN_POINT('Ctrl Pts',(15.1211545887425,0.000250233060073018,
4.59495282954609));
#25888=CARTESIAN_POINT('Ctrl Pts',(15.135938272063,-0.18295950063263,4.59398211075496));
#25889=CARTESIAN_POINT('Ctrl Pts',(15.1507219553836,-0.367002343096231,
4.50294888365168));
#25890=CARTESIAN_POINT('Ctrl Pts',(15.1655056387041,-0.476631971954554,
4.35629051265579));
#25891=CARTESIAN_POINT('Ctrl Pts',(15.1814109173917,-0.594578884209397,
4.19850559451431));
#25892=CARTESIAN_POINT('Ctrl Pts',(15.1973161960793,-0.626393242576541,
3.97633512612291));
#25893=CARTESIAN_POINT('Ctrl Pts',(15.2132214747669,-0.557467239648298,
3.79179038730953));
#25894=CARTESIAN_POINT('Ctrl Pts',(15.2291267534545,-0.488541236720055,
3.60724564849615));
#25895=CARTESIAN_POINT('Ctrl Pts',(15.2450320321422,-0.318874872496425,
3.46032663926078));
#25896=CARTESIAN_POINT('Ctrl Pts',(15.2609373108298,-0.126371763436977,
3.41849235301362));
#25897=CARTESIAN_POINT('Ctrl Pts',(15.2768425895174,0.0661313456224706,
3.37665806676646));
#25898=CARTESIAN_POINT('Ctrl Pts',(15.292747868205,0.281471199517752,3.4399085035075));
#25899=CARTESIAN_POINT('Ctrl Pts',(15.3086531468926,0.420772847618048,3.57920173859056));
#25900=CARTESIAN_POINT('Ctrl Pts',(15.3245584255802,0.560074495718348,3.71849497367363));
#25901=CARTESIAN_POINT('Ctrl Pts',(15.3404637042678,0.623337938023671,3.9338310070987));
#25902=CARTESIAN_POINT('Ctrl Pts',(15.3563689829554,0.581515278282945,4.12633664243329));
#25903=CARTESIAN_POINT('Ctrl Pts',(15.3722742616431,0.53969261854222,4.31884227776789));
#25904=CARTESIAN_POINT('Ctrl Pts',(15.3881795403307,0.392783856755445,4.48851751501199));
#25905=CARTESIAN_POINT('Ctrl Pts',(15.4040848190183,0.208243281137944,4.55745466359042));
#25906=CARTESIAN_POINT('Ctrl Pts',(15.4097747422597,0.142226097106806,4.58211610408423));
#25907=CARTESIAN_POINT('Ctrl Pts',(15.4154646655011,0.0713929250243718,
4.593885435962));
#25908=CARTESIAN_POINT('Ctrl Pts',(15.4211545887425,0.000414092275955974,
4.59343115273787));
#25909=CARTESIAN_POINT('Origin',(4.,0.,4.));
#25910=CARTESIAN_POINT('',(15.8288454112575,-0.000332254705457391,4.59484959654372));
#25911=CARTESIAN_POINT('',(15.7211545887425,-0.000419917270904514,4.59344262983929));
#25912=CARTESIAN_POINT('',(4.,-7.27562663373442E-17,4.5941));
#25913=CARTESIAN_POINT('Ctrl Pts',(15.8288454112575,-0.000332254705457391,
4.59484959654372));
#25914=CARTESIAN_POINT('Ctrl Pts',(15.814487640426,0.177680873019276,4.5936575613883));
#25915=CARTESIAN_POINT('Ctrl Pts',(15.8001298695944,0.356683508224643,4.50844978272675));
#25916=CARTESIAN_POINT('Ctrl Pts',(15.7857720987628,0.466927807092597,4.36891650689757));
#25917=CARTESIAN_POINT('Ctrl Pts',(15.7698668200752,0.589054446233417,4.21434406913608));
#25918=CARTESIAN_POINT('Ctrl Pts',(15.7539615413876,0.626802179063893,3.99310442736787));
#25919=CARTESIAN_POINT('Ctrl Pts',(15.7380562627,0.562838843643149,3.80678146521555));
#25920=CARTESIAN_POINT('Ctrl Pts',(15.7221509840123,0.498875508222402,3.62045850306322));
#25921=CARTESIAN_POINT('Ctrl Pts',(15.7062457053247,0.333201104550436,3.46905222052678));
#25922=CARTESIAN_POINT('Ctrl Pts',(15.6903404266371,0.141886309687413,3.42208197707538));
#25923=CARTESIAN_POINT('Ctrl Pts',(15.6744351479495,-0.0494284851756215,
3.37511173362399));
#25924=CARTESIAN_POINT('Ctrl Pts',(15.6585298692619,-0.266383671229707,
3.43257752925765));
#25925=CARTESIAN_POINT('Ctrl Pts',(15.6426245905743,-0.409362605655794,
3.5680935017987));
#25926=CARTESIAN_POINT('Ctrl Pts',(15.6267193118867,-0.552341540081869,
3.70360947433975));
#25927=CARTESIAN_POINT('Ctrl Pts',(15.6108140331991,-0.621344222879956,
3.9171756237882));
#25928=CARTESIAN_POINT('Ctrl Pts',(15.5949087545115,-0.584687541371933,
4.11073140955597));
#25929=CARTESIAN_POINT('Ctrl Pts',(15.5790034758238,-0.548030859863907,
4.30428719532377));
#25930=CARTESIAN_POINT('Ctrl Pts',(15.5630981971362,-0.405714814049763,
4.47783261741089));
#25931=CARTESIAN_POINT('Ctrl Pts',(15.5471929184486,-0.223084911271984,
4.55168296009627));
#25932=CARTESIAN_POINT('Ctrl Pts',(15.5410770827183,-0.152860773312716,
4.58007960584922));
#25933=CARTESIAN_POINT('Ctrl Pts',(15.5349612469879,-0.0766761255292402,
4.5937360717991));
#25934=CARTESIAN_POINT('Ctrl Pts',(15.5288454112575,-0.000350670266729247,
4.59332700645389));
#25935=CARTESIAN_POINT('Ctrl Pts',(15.4211545887425,0.000414092275955974,
4.59343115273787));
#25936=CARTESIAN_POINT('Ctrl Pts',(15.4313699441887,-0.12701715326484,4.59261555920332));
#25937=CARTESIAN_POINT('Ctrl Pts',(15.4415852996349,-0.254917899718674,
4.55240018390688));
#25938=CARTESIAN_POINT('Ctrl Pts',(15.4518006550811,-0.356261725310785,
4.47665348962993));
#25939=CARTESIAN_POINT('Ctrl Pts',(15.4677059337687,-0.514053766693778,
4.35871610717824));
#25940=CARTESIAN_POINT('Ctrl Pts',(15.4836112124564,-0.607465460011524,
4.15464228236211));
#25941=CARTESIAN_POINT('Ctrl Pts',(15.499516491144,-0.593606107615349,3.95813408188558));
#25942=CARTESIAN_POINT('Ctrl Pts',(15.5154217698316,-0.579746755219174,
3.76162588140906));
#25943=CARTESIAN_POINT('Ctrl Pts',(15.5313270485192,-0.458616357109098,
3.57268330527213));
#25944=CARTESIAN_POINT('Ctrl Pts',(15.5472323272068,-0.285832867492734,
3.47806079093568));
#25945=CARTESIAN_POINT('Ctrl Pts',(15.5631376058944,-0.113049377876356,
3.38343827659922));
#25946=CARTESIAN_POINT('Ctrl Pts',(15.579042884582,0.111387203246309,3.38313582406324));
#25947=CARTESIAN_POINT('Ctrl Pts',(15.5949481632696,0.284425092952457,3.47729230673655));
#25948=CARTESIAN_POINT('Ctrl Pts',(15.6108534419572,0.457462982658595,3.57144878940986));
#25949=CARTESIAN_POINT('Ctrl Pts',(15.6267587206449,0.579102180948212,3.76006420729246));
#25950=CARTESIAN_POINT('Ctrl Pts',(15.6426639993325,0.593491114096805,3.95653434015292));
#25951=CARTESIAN_POINT('Ctrl Pts',(15.6585692780201,0.607880047245398,4.15300447301339));
#25952=CARTESIAN_POINT('Ctrl Pts',(15.6744745567077,0.515018715252963,4.35732932085173));
#25953=CARTESIAN_POINT('Ctrl Pts',(15.6903798353953,0.357545113131455,4.47569155781202));
#25954=CARTESIAN_POINT('Ctrl Pts',(15.700638086511,0.255981111243369,4.55203033647815));
#25955=CARTESIAN_POINT('Ctrl Pts',(15.7108963376268,0.127540214881222,4.59261107697802));
#25956=CARTESIAN_POINT('Ctrl Pts',(15.7211545887425,-0.000419917270904514,
4.59344262983929));
#25957=CARTESIAN_POINT('Origin',(4.,0.,4.));
#25958=CARTESIAN_POINT('',(16.1288454112575,0.000520203518568921,4.59435747030618));
#25959=CARTESIAN_POINT('',(16.0211545887425,-0.00024144267326323,4.59496181546483));
#25960=CARTESIAN_POINT('',(4.,-7.27562663373442E-17,4.5941));
#25961=CARTESIAN_POINT('Ctrl Pts',(16.1288454112575,0.000520203518568921,
4.59435747030618));
#25962=CARTESIAN_POINT('Ctrl Pts',(16.1258245912393,0.0380542554257849,
4.59470210862833));
#25963=CARTESIAN_POINT('Ctrl Pts',(16.122803771221,0.0755288363057283,4.59145263304759));
#25964=CARTESIAN_POINT('Ctrl Pts',(16.1197829512027,0.112271568866026,4.58439375503351));
#25965=CARTESIAN_POINT('Ctrl Pts',(16.1038776725151,0.305730099191281,4.54722721702202));
#25966=CARTESIAN_POINT('Ctrl Pts',(16.0879723938275,0.478899942385972,4.40445440507416));
#25967=CARTESIAN_POINT('Ctrl Pts',(16.0720671151398,0.55226883266698,4.22163055421683));
#25968=CARTESIAN_POINT('Ctrl Pts',(16.0561618364522,0.625637722947984,4.03880670335952));
#25969=CARTESIAN_POINT('Ctrl Pts',(16.0402565577646,0.599205660315318,3.81593181359275));
#25970=CARTESIAN_POINT('Ctrl Pts',(16.024351279077,0.485109129681553,3.65534060523843));
#25971=CARTESIAN_POINT('Ctrl Pts',(16.0084460003894,0.371012599047788,3.4947493968841));
#25972=CARTESIAN_POINT('Ctrl Pts',(15.9925407217018,0.169251600412921,3.39644186994223));
#25973=CARTESIAN_POINT('Ctrl Pts',(15.9766354430142,-0.0275337514538456,
3.40555668173602));
#25974=CARTESIAN_POINT('Ctrl Pts',(15.9607301643265,-0.224319103320618,
3.41467149352982));
#25975=CARTESIAN_POINT('Ctrl Pts',(15.9448248856389,-0.416128808419276,
3.53120864405929));
#25976=CARTESIAN_POINT('Ctrl Pts',(15.9289196069513,-0.514891964967956,
3.70165920408156));
#25977=CARTESIAN_POINT('Ctrl Pts',(15.9130143282637,-0.613655121516638,
3.87210976410384));
#25978=CARTESIAN_POINT('Ctrl Pts',(15.8971090495761,-0.619371729515322,
4.09647373361892));
#25979=CARTESIAN_POINT('Ctrl Pts',(15.8812037708885,-0.52941696442075,4.27173266988224));
#25980=CARTESIAN_POINT('Ctrl Pts',(15.8652984922009,-0.439462199326184,
4.44699160614554));
#25981=CARTESIAN_POINT('Ctrl Pts',(15.8493932135132,-0.25383606113837,4.57314550915708));
#25982=CARTESIAN_POINT('Ctrl Pts',(15.8334879348256,-0.0577702193188812,
4.59226984378546));
#25983=CARTESIAN_POINT('Ctrl Pts',(15.8319404269696,-0.0386939468137543,
4.59413055045147));
#25984=CARTESIAN_POINT('Ctrl Pts',(15.8303929191136,-0.0195188482833839,
4.59497807636063));
#25985=CARTESIAN_POINT('Ctrl Pts',(15.8288454112575,-0.000332254705457391,
4.59484959654372));
#25986=CARTESIAN_POINT('Ctrl Pts',(15.7211545887425,-0.000419917270904514,
4.59344262983929));
#25987=CARTESIAN_POINT('Ctrl Pts',(15.7268016163144,-0.0708602278282204,
4.59390038836772));
#25988=CARTESIAN_POINT('Ctrl Pts',(15.7324486438863,-0.141154849878182,
4.58231274148771));
#25989=CARTESIAN_POINT('Ctrl Pts',(15.7380956714582,-0.206740066761224,
4.55801389847688));
#25990=CARTESIAN_POINT('Ctrl Pts',(15.7540009501458,-0.391465772281827,
4.48957437609924));
#25991=CARTESIAN_POINT('Ctrl Pts',(15.7699062288334,-0.538831311072463,
4.32029570526172));
#25992=CARTESIAN_POINT('Ctrl Pts',(15.785811507521,-0.58117266224226,4.12790349002296));
#25993=CARTESIAN_POINT('Ctrl Pts',(15.8017167862086,-0.62351401341206,3.93551127478418));
#25994=CARTESIAN_POINT('Ctrl Pts',(15.8176220648962,-0.560831176961022,
3.72000551514415));
#25995=CARTESIAN_POINT('Ctrl Pts',(15.8335273435838,-0.421905459495345,
3.58033733863277));
#25996=CARTESIAN_POINT('Ctrl Pts',(15.8494326222715,-0.282979742029676,
3.44066916212139));
#25997=CARTESIAN_POINT('Ctrl Pts',(15.8653379009591,-0.0678111435493865,
3.37683856873865));
#25998=CARTESIAN_POINT('Ctrl Pts',(15.8812431796467,0.124804018556085,3.41815386651619));
#25999=CARTESIAN_POINT('Ctrl Pts',(15.8971484583343,0.317419180661557,3.45946916429373));
#26000=CARTESIAN_POINT('Ctrl Pts',(15.9130537370219,0.487480906392202,3.60593035323155));
#26001=CARTESIAN_POINT('Ctrl Pts',(15.9289590157095,0.556904046010802,3.79028865163133));
#26002=CARTESIAN_POINT('Ctrl Pts',(15.9448642943971,0.6263271856294,3.9746469500311));
#26003=CARTESIAN_POINT('Ctrl Pts',(15.9607695730847,0.595111739135951,4.19690235789283));
#26004=CARTESIAN_POINT('Ctrl Pts',(15.9766748517723,0.477590518943614,4.35500459477727));
#26005=CARTESIAN_POINT('Ctrl Pts',(15.9915014307624,0.368039615220995,4.50238430120742));
#26006=CARTESIAN_POINT('Ctrl Pts',(16.0063280097524,0.18349252241573,4.59401752470064));
#26007=CARTESIAN_POINT('Ctrl Pts',(16.0211545887425,-0.00024144267326323,
4.59496181546483));
#26008=CARTESIAN_POINT('Origin',(4.,0.,4.));
#26009=CARTESIAN_POINT('',(16.4288454112575,7.48704377684928E-5,4.59312461313858));
#26010=CARTESIAN_POINT('',(16.3211545887425,0.000543344619121817,4.59417988242975));
#26011=CARTESIAN_POINT('',(4.,-7.27562663373442E-17,4.5941));
#26012=CARTESIAN_POINT('Ctrl Pts',(16.4288454112575,7.48704377684928E-5,
4.59312461313858));
#26013=CARTESIAN_POINT('Ctrl Pts',(16.4212562633649,0.0948679978941589,
4.5932308806522));
#26014=CARTESIAN_POINT('Ctrl Pts',(16.4136671154723,0.189615837117123,4.57184094704105));
#26015=CARTESIAN_POINT('Ctrl Pts',(16.4060779675797,0.273126642574496,4.52869916135151));
#26016=CARTESIAN_POINT('Ctrl Pts',(16.3901726888921,0.448147956300534,4.43828293357696));
#26017=CARTESIAN_POINT('Ctrl Pts',(16.3742674102045,0.573812330828296,4.25232504748949));
#26018=CARTESIAN_POINT('Ctrl Pts',(16.3583621315169,0.592420001795879,4.05620949715111));
#26019=CARTESIAN_POINT('Ctrl Pts',(16.3424568528292,0.611027672763462,3.86009394681272));
#26020=CARTESIAN_POINT('Ctrl Pts',(16.3265515741416,0.522578640170867,3.6538207322234));
#26021=CARTESIAN_POINT('Ctrl Pts',(16.310646295454,0.367684957814641,3.53210178682255));
#26022=CARTESIAN_POINT('Ctrl Pts',(16.2947410167664,0.212791275458425,3.4103828414217));
#26023=CARTESIAN_POINT('Ctrl Pts',(16.2788357380788,-0.00854705666138705,
3.3732181652093));
#26024=CARTESIAN_POINT('Ctrl Pts',(16.2629304593912,-0.19470084048803,3.43767220519428));
#26025=CARTESIAN_POINT('Ctrl Pts',(16.2470251807036,-0.380854624314662,
3.50212624517926));
#26026=CARTESIAN_POINT('Ctrl Pts',(16.231119902016,-0.531823859848111,3.66819900136163));
#26027=CARTESIAN_POINT('Ctrl Pts',(16.2152146233283,-0.578289861113055,
3.85963689006134));
#26028=CARTESIAN_POINT('Ctrl Pts',(16.1993093446407,-0.624755862378002,
4.05107477876107));
#26029=CARTESIAN_POINT('Ctrl Pts',(16.1834040659531,-0.566718629374431,
4.26787779997815));
#26030=CARTESIAN_POINT('Ctrl Pts',(16.1674987872655,-0.430826404144746,
4.41049917854914));
#26031=CARTESIAN_POINT('Ctrl Pts',(16.1546143285962,-0.320743594918802,
4.52603310245269));
#26032=CARTESIAN_POINT('Ctrl Pts',(16.1417298699269,-0.159570744489656,
4.592887512417));
#26033=CARTESIAN_POINT('Ctrl Pts',(16.1288454112575,0.000520203518568921,
4.59435747030618));
#26034=CARTESIAN_POINT('Ctrl Pts',(16.0211545887425,-0.00024144267326323,
4.59496181546483));
#26035=CARTESIAN_POINT('Ctrl Pts',(16.0222332884401,-0.0136089074611732,
4.59503051682625));
#26036=CARTESIAN_POINT('Ctrl Pts',(16.0233119881376,-0.0269720681925484,
4.59461918253551));
#26037=CARTESIAN_POINT('Ctrl Pts',(16.0243906878352,-0.0403017303441999,
4.59371435609144));
#26038=CARTESIAN_POINT('Ctrl Pts',(16.0402959665228,-0.236845765548457,
4.58037281461397));
#26039=CARTESIAN_POINT('Ctrl Pts',(16.0562012452104,-0.426106842065734,
4.45974066575184));
#26040=CARTESIAN_POINT('Ctrl Pts',(16.072106523898,-0.521184280535122,4.2872070887372));
#26041=CARTESIAN_POINT('Ctrl Pts',(16.0880118025856,-0.616261719004504,
4.11467351172257));
#26042=CARTESIAN_POINT('Ctrl Pts',(16.1039170812732,-0.61715551942601,3.89023850655542));
#26043=CARTESIAN_POINT('Ctrl Pts',(16.1198223599609,-0.523455286459661,
3.71695313254649));
#26044=CARTESIAN_POINT('Ctrl Pts',(16.1357276386485,-0.429755053493313,
3.54366775853756));
#26045=CARTESIAN_POINT('Ctrl Pts',(16.1516329173361,-0.241460787139106,
3.42153201568684));
#26046=CARTESIAN_POINT('Ctrl Pts',(16.1675381960237,-0.045029248433429,
3.40662546997421));
#26047=CARTESIAN_POINT('Ctrl Pts',(16.1834434747113,0.151402290272254,3.39171892426158));
#26048=CARTESIAN_POINT('Ctrl Pts',(16.1993487533989,0.355971101329402,3.48404157568705));
#26049=CARTESIAN_POINT('Ctrl Pts',(16.2152540320865,0.474747841293266,3.64120276856532));
#26050=CARTESIAN_POINT('Ctrl Pts',(16.2311593107741,0.593524581257127,3.79836396144359));
#26051=CARTESIAN_POINT('Ctrl Pts',(16.2470645894618,0.626509250127697,4.02036369577466));
#26052=CARTESIAN_POINT('Ctrl Pts',(16.2629698681494,0.558556683425868,4.20526908558792));
#26053=CARTESIAN_POINT('Ctrl Pts',(16.278875146837,0.490604116724039,4.39017447540119));
#26054=CARTESIAN_POINT('Ctrl Pts',(16.2947804255246,0.32171431444981,4.53798552069667));
#26055=CARTESIAN_POINT('Ctrl Pts',(16.3106857042122,0.129434328669215,4.58083364284428));
#26056=CARTESIAN_POINT('Ctrl Pts',(16.314175332389,0.0872479785030607,4.5902345478711));
#26057=CARTESIAN_POINT('Ctrl Pts',(16.3176649605657,0.0439357035691123,
4.5945828907904));
#26058=CARTESIAN_POINT('Ctrl Pts',(16.3211545887425,0.000543344619121817,
4.59417988242975));
#26059=CARTESIAN_POINT('Origin',(4.,0.,4.));
#26060=CARTESIAN_POINT('',(16.7288454112575,-0.000548108868865471,4.59408180714414));
#26061=CARTESIAN_POINT('',(16.6211545887425,-2.1752937549985E-5,4.5931168278739));
#26062=CARTESIAN_POINT('',(4.,-7.27562663373442E-17,4.5941));
#26063=CARTESIAN_POINT('Ctrl Pts',(16.7288454112575,-0.000548108868865471,
4.59408180714414));
#26064=CARTESIAN_POINT('Ctrl Pts',(16.7166879354906,0.15068989439403,4.59268722311157));
#26065=CARTESIAN_POINT('Ctrl Pts',(16.7045304597237,0.302891836883802,4.53390177381835));
#26066=CARTESIAN_POINT('Ctrl Pts',(16.6923729839567,0.411632901649024,4.42974331917764));
#26067=CARTESIAN_POINT('Ctrl Pts',(16.6764677052691,0.553895734249677,4.29347578465895));
#26068=CARTESIAN_POINT('Ctrl Pts',(16.6605624265815,0.621772048174623,4.07954898308531));
#26069=CARTESIAN_POINT('Ctrl Pts',(16.6446571478939,0.58409591167956,3.88618905124272));
#26070=CARTESIAN_POINT('Ctrl Pts',(16.6287518692063,0.546419775184499,3.69282911940014));
#26071=CARTESIAN_POINT('Ctrl Pts',(16.6128465905187,0.403191188269443,3.52003605728863));
#26072=CARTESIAN_POINT('Ctrl Pts',(16.596941311831,0.220174658543969,3.44714912875817));
#26073=CARTESIAN_POINT('Ctrl Pts',(16.5810360331434,0.0371581288184754,
3.37426220022769));
#26074=CARTESIAN_POINT('Ctrl Pts',(16.5651307544558,-0.185646343717467,
3.40128140527831));
#26075=CARTESIAN_POINT('Ctrl Pts',(16.5492254757682,-0.34593637135519,3.51580066803907));
#26076=CARTESIAN_POINT('Ctrl Pts',(16.5333201970806,-0.506226398992903,
3.63031993079982));
#26077=CARTESIAN_POINT('Ctrl Pts',(16.517414918393,-0.604001981732426,3.83233925127069));
#26078=CARTESIAN_POINT('Ctrl Pts',(16.5015096397054,-0.594368708523554,
4.02909990422408));
#26079=CARTESIAN_POINT('Ctrl Pts',(16.4856043610178,-0.584735435314682,
4.22586055717748));
#26080=CARTESIAN_POINT('Ctrl Pts',(16.4696990823301,-0.467693306157413,
4.4173625426134));
#26081=CARTESIAN_POINT('Ctrl Pts',(16.4537938036425,-0.296983115116624,
4.51567625060054));
#26082=CARTESIAN_POINT('Ctrl Pts',(16.4454776728475,-0.20772669247752,4.56707991793767));
#26083=CARTESIAN_POINT('Ctrl Pts',(16.4371615420525,-0.103798720846626,
4.59300816600183));
#26084=CARTESIAN_POINT('Ctrl Pts',(16.4288454112575,7.48704377684928E-5,
4.59312461313858));
#26085=CARTESIAN_POINT('Ctrl Pts',(16.3211545887425,0.000543344619121817,
4.59417988242975));
#26086=CARTESIAN_POINT('Ctrl Pts',(16.3335702392533,-0.153841115924154,
4.59274603025257));
#26087=CARTESIAN_POINT('Ctrl Pts',(16.3459858897642,-0.309239316255332,
4.53116741914846));
#26088=CARTESIAN_POINT('Ctrl Pts',(16.3584015402751,-0.418549561707542,
4.42300972860235));
#26089=CARTESIAN_POINT('Ctrl Pts',(16.3743068189627,-0.558583297016706,
4.28445249321304));
#26090=CARTESIAN_POINT('Ctrl Pts',(16.3902120976503,-0.622980598348072,
4.06945282343469));
#26091=CARTESIAN_POINT('Ctrl Pts',(16.4061173763379,-0.582172949355422,
3.87672947174358));
#26092=CARTESIAN_POINT('Ctrl Pts',(16.4220226550255,-0.541365300362771,
3.68400612005246));
#26093=CARTESIAN_POINT('Ctrl Pts',(16.4379279337131,-0.395352701046104,
3.5135590864486));
#26094=CARTESIAN_POINT('Ctrl Pts',(16.4538332124007,-0.211177959727979,
3.44365043774355));
#26095=CARTESIAN_POINT('Ctrl Pts',(16.4697384910883,-0.0270032184098532,
3.37374178903851));
#26096=CARTESIAN_POINT('Ctrl Pts',(16.485643769776,0.195333664909731,3.40437152523229));
#26097=CARTESIAN_POINT('Ctrl Pts',(16.5015490484636,0.353744999708243,3.52147576730199));
#26098=CARTESIAN_POINT('Ctrl Pts',(16.5174543271512,0.512156334506764,3.63858000937169));
#26099=CARTESIAN_POINT('Ctrl Pts',(16.5333596058388,0.606642120784206,3.84215875731731));
#26100=CARTESIAN_POINT('Ctrl Pts',(16.5492648845264,0.59381848284593,4.03873726278877));
#26101=CARTESIAN_POINT('Ctrl Pts',(16.565170163214,0.580994844907655,4.23531576826023));
#26102=CARTESIAN_POINT('Ctrl Pts',(16.5810754419016,0.460861782753675,4.42489403125753));
#26103=CARTESIAN_POINT('Ctrl Pts',(16.5969807205892,0.288579316114369,4.52042573380721));
#26104=CARTESIAN_POINT('Ctrl Pts',(16.6050386766403,0.201297315476928,4.56882414767653));
#26105=CARTESIAN_POINT('Ctrl Pts',(16.6130966326914,0.100630370301649,4.59308406930439));
#26106=CARTESIAN_POINT('Ctrl Pts',(16.6211545887425,-2.1752937549985E-5,
4.5931168278739));
#26107=CARTESIAN_POINT('Origin',(4.,0.,4.));
#26108=CARTESIAN_POINT('',(17.0288454112575,0.000186802344652959,4.59500977980842));
#26109=CARTESIAN_POINT('',(16.9211545887425,-0.000535257393875686,4.59425998651214));
#26110=CARTESIAN_POINT('',(4.,-7.27562663373442E-17,4.5941));
#26111=CARTESIAN_POINT('Ctrl Pts',(17.0288454112575,0.000186802344652959,
4.59500977980842));
#26112=CARTESIAN_POINT('Ctrl Pts',(17.0280248863039,0.0103527338555297,
4.59505157132578));
#26113=CARTESIAN_POINT('Ctrl Pts',(17.0272043613502,0.0205166685362397,
4.5948136789481));
#26114=CARTESIAN_POINT('Ctrl Pts',(17.0263838363966,0.0306658549750798,
4.59428997251885));
#26115=CARTESIAN_POINT('Ctrl Pts',(17.010478557709,0.227400443050786,4.58413830477164));
#26116=CARTESIAN_POINT('Ctrl Pts',(16.9945732790214,0.418593379366704,4.46659200952389));
#26117=CARTESIAN_POINT('Ctrl Pts',(16.9786680003338,0.516456956272638,4.29562337257973));
#26118=CARTESIAN_POINT('Ctrl Pts',(16.9627627216462,0.614320533178566,4.12465473563558));
#26119=CARTESIAN_POINT('Ctrl Pts',(16.9468574429585,0.618854750674521,3.90026375699502));
#26120=CARTESIAN_POINT('Ctrl Pts',(16.9309521642709,0.527977687913284,3.72548128085037));
#26121=CARTESIAN_POINT('Ctrl Pts',(16.9150468855833,0.437100625152047,3.55069880470573));
#26122=CARTESIAN_POINT('Ctrl Pts',(16.8991416068957,0.25081228213362,3.42552483105699));
#26123=CARTESIAN_POINT('Ctrl Pts',(16.8832363282081,0.054648384762208,3.40743395292956));
#26124=CARTESIAN_POINT('Ctrl Pts',(16.8673310495205,-0.141515512609204,
3.38934307480212));
#26125=CARTESIAN_POINT('Ctrl Pts',(16.8514257708328,-0.347554964333599,
3.47833529219599));
#26126=CARTESIAN_POINT('Ctrl Pts',(16.8355204921452,-0.468865370989487,
3.63354914383413));
#26127=CARTESIAN_POINT('Ctrl Pts',(16.8196152134576,-0.590175777645383,
3.78876299547228));
#26128=CARTESIAN_POINT('Ctrl Pts',(16.80370993477,-0.62675713923276,4.01019848135471));
#26129=CARTESIAN_POINT('Ctrl Pts',(16.7878046560824,-0.561812842140477,
4.19618179452704));
#26130=CARTESIAN_POINT('Ctrl Pts',(16.7718993773948,-0.496868545048197,
4.38216510769936));
#26131=CARTESIAN_POINT('Ctrl Pts',(16.7559940987072,-0.330398589276266,
4.53269624816158));
#26132=CARTESIAN_POINT('Ctrl Pts',(16.7400888200196,-0.138838935752124,
4.57865768466082));
#26133=CARTESIAN_POINT('Ctrl Pts',(16.7363410170989,-0.0937012275068688,
4.58948769960953));
#26134=CARTESIAN_POINT('Ctrl Pts',(16.7325932141782,-0.0471704703862807,
4.59451171761327));
#26135=CARTESIAN_POINT('Ctrl Pts',(16.7288454112575,-0.000548108868865471,
4.59408180714414));
#26136=CARTESIAN_POINT('Ctrl Pts',(16.6211545887425,-2.1752937549985E-5,
4.5931168278739));
#26137=CARTESIAN_POINT('Ctrl Pts',(16.629001911379,-0.0980428491191961,
4.59314873014073));
#26138=CARTESIAN_POINT('Ctrl Pts',(16.6368492340155,-0.196049888122182,
4.57020350190738));
#26139=CARTESIAN_POINT('Ctrl Pts',(16.6446965566521,-0.281666676968544,
4.52419924569128));
#26140=CARTESIAN_POINT('Ctrl Pts',(16.6606018353397,-0.455198332287519,
4.43095591292362));
#26141=CARTESIAN_POINT('Ctrl Pts',(16.6765071140273,-0.577829771800838,
4.24298410528626));
#26142=CARTESIAN_POINT('Ctrl Pts',(16.6924123927149,-0.593253826592341,
4.0465925244149));
#26143=CARTESIAN_POINT('Ctrl Pts',(16.7083176714025,-0.608677881383846,
3.85020094354353));
#26144=CARTESIAN_POINT('Ctrl Pts',(16.7242229500901,-0.516894551453523,
3.64538958943816));
#26145=CARTESIAN_POINT('Ctrl Pts',(16.7401282287778,-0.360046858872914,
3.52619917105016));
#26146=CARTESIAN_POINT('Ctrl Pts',(16.7560335074654,-0.203199166292313,
3.40700875266216));
#26147=CARTESIAN_POINT('Ctrl Pts',(16.771938786153,0.0187128889385656,3.37343926999153));
#26148=CARTESIAN_POINT('Ctrl Pts',(16.7878440648406,0.203796679382533,3.44090440927292));
#26149=CARTESIAN_POINT('Ctrl Pts',(16.8037493435282,0.388880469826499,3.50836954855431));
#26150=CARTESIAN_POINT('Ctrl Pts',(16.8196546222158,0.537135995483554,3.67686930978772));
#26151=CARTESIAN_POINT('Ctrl Pts',(16.8355599009034,0.58049059114602,3.86903573125179));
#26152=CARTESIAN_POINT('Ctrl Pts',(16.851465179591,0.623845186808487,4.06120215271587));
#26153=CARTESIAN_POINT('Ctrl Pts',(16.8673704582787,0.562298852476364,4.2770352344106));
#26154=CARTESIAN_POINT('Ctrl Pts',(16.8832757369663,0.424111061064287,4.41743355636644));
#26155=CARTESIAN_POINT('Ctrl Pts',(16.8959020208917,0.314411738992559,4.5288876912157));
#26156=CARTESIAN_POINT('Ctrl Pts',(16.9085283048171,0.156414067554279,4.59280392009262));
#26157=CARTESIAN_POINT('Ctrl Pts',(16.9211545887425,-0.000535257393875686,
4.59425998651214));
#26158=CARTESIAN_POINT('Origin',(4.,0.,4.));
#26159=CARTESIAN_POINT('',(17.3288454112575,0.000452601584348983,4.59351524744837));
#26160=CARTESIAN_POINT('',(17.2211545887425,0.000283723793354941,4.5949151055343));
#26161=CARTESIAN_POINT('',(4.,-7.27562663373442E-17,4.5941));
#26162=CARTESIAN_POINT('Ctrl Pts',(17.3288454112575,0.000452601584348983,
4.59351524744837));
#26163=CARTESIAN_POINT('Ctrl Pts',(17.3234565584296,0.0676518012035294,
4.59398979695312));
#26164=CARTESIAN_POINT('Ctrl Pts',(17.3180677056016,0.134706745978521,4.58346365752876));
#26165=CARTESIAN_POINT('Ctrl Pts',(17.3126788527736,0.197661386620268,4.56129398922237));
#26166=CARTESIAN_POINT('Ctrl Pts',(17.296773574086,0.383472937993069,4.49585988588324));
#26167=CARTESIAN_POINT('Ctrl Pts',(17.2808682953984,0.533564938357213,4.32899388620009));
#26168=CARTESIAN_POINT('Ctrl Pts',(17.2649630167108,0.579021491014364,4.13731379770915));
#26169=CARTESIAN_POINT('Ctrl Pts',(17.2490577380232,0.624478043671518,3.94563370921821));
#26170=CARTESIAN_POINT('Ctrl Pts',(17.2331524593355,0.565299148621668,3.72913953191949));
#26171=CARTESIAN_POINT('Ctrl Pts',(17.2172471806479,0.428657250819126,3.58723623291525));
#26172=CARTESIAN_POINT('Ctrl Pts',(17.2013419019603,0.292015353016592,3.44533293391101));
#26173=CARTESIAN_POINT('Ctrl Pts',(17.1854366232727,0.0779104524613767,
3.37802051320125));
#26174=CARTESIAN_POINT('Ctrl Pts',(17.1695313445851,-0.115349538542919,
3.41620598662221));
#26175=CARTESIAN_POINT('Ctrl Pts',(17.1536260658975,-0.308609529547215,
3.45439146004317));
#26176=CARTESIAN_POINT('Ctrl Pts',(17.1377207872099,-0.48102461100059,3.59807482759486));
#26177=CARTESIAN_POINT('Ctrl Pts',(17.1218155085223,-0.553429071780215,
3.78128276563952));
#26178=CARTESIAN_POINT('Ctrl Pts',(17.1059102298347,-0.625833532559839,
3.96449070368418));
#26179=CARTESIAN_POINT('Ctrl Pts',(17.090004951147,-0.598227372665711,4.18722321222181));
#26180=CARTESIAN_POINT('Ctrl Pts',(17.0740996724594,-0.483286172800906,
4.34721094636728));
#26181=CARTESIAN_POINT('Ctrl Pts',(17.0590149187255,-0.374274584390508,
4.4989451987145));
#26182=CARTESIAN_POINT('Ctrl Pts',(17.0439301649915,-0.186706445247169,
4.59424147319602));
#26183=CARTESIAN_POINT('Ctrl Pts',(17.0288454112575,0.000186802344652959,
4.59500977980842));
#26184=CARTESIAN_POINT('Ctrl Pts',(16.9211545887425,-0.000535257393875686,
4.59425998651214));
#26185=CARTESIAN_POINT('Ctrl Pts',(16.9244335835047,-0.0412943609811605,
4.59463812105998));
#26186=CARTESIAN_POINT('Ctrl Pts',(16.9277125782669,-0.0819827620002526,
4.59080381827239));
#26187=CARTESIAN_POINT('Ctrl Pts',(16.9309915730291,-0.121736182180322,
4.58249572362891));
#26188=CARTESIAN_POINT('Ctrl Pts',(16.9468968517167,-0.31456638552074,4.54219600671859));
#26189=CARTESIAN_POINT('Ctrl Pts',(16.9628021304043,-0.485397543709551,
4.39663301068103));
#26190=CARTESIAN_POINT('Ctrl Pts',(16.978707409092,-0.555791216176751,4.21264310503418));
#26191=CARTESIAN_POINT('Ctrl Pts',(16.9946126877796,-0.626184888643955,
4.02865319938731));
#26192=CARTESIAN_POINT('Ctrl Pts',(17.0105179664672,-0.596141075389537,
3.80623638413113));
#26193=CARTESIAN_POINT('Ctrl Pts',(17.0264232451548,-0.479454624411006,
3.64751705115182));
#26194=CARTESIAN_POINT('Ctrl Pts',(17.0423285238424,-0.362768173432475,
3.48879771817251));
#26195=CARTESIAN_POINT('Ctrl Pts',(17.05823380253,-0.159439084729831,3.39377586747005));
#26196=CARTESIAN_POINT('Ctrl Pts',(17.0741390812176,0.0371725263090214,
3.40608151284405));
#26197=CARTESIAN_POINT('Ctrl Pts',(17.0900443599052,0.233784137347885,3.41838715821804));
#26198=CARTESIAN_POINT('Ctrl Pts',(17.1059496385929,0.423678270722955,3.5380202996685));
#26199=CARTESIAN_POINT('Ctrl Pts',(17.1218549172805,0.519663574146654,3.71005045990219));
#26200=CARTESIAN_POINT('Ctrl Pts',(17.1377601959681,0.615648877570348,3.88208062013586));
#26201=CARTESIAN_POINT('Ctrl Pts',(17.1536654746557,0.617725351042682,4.10650779915277));
#26202=CARTESIAN_POINT('Ctrl Pts',(17.1695707533433,0.524939565793509,4.28028453107927));
#26203=CARTESIAN_POINT('Ctrl Pts',(17.1854760320309,0.432153780544336,4.45406126300578));
#26204=CARTESIAN_POINT('Ctrl Pts',(17.2013813107185,0.244505736573655,4.5771875478419));
#26205=CARTESIAN_POINT('Ctrl Pts',(17.2172865894061,0.0481554769387473,
4.59312900463441));
#26206=CARTESIAN_POINT('Ctrl Pts',(17.2185759225182,0.0322386925622284,
4.59442127046022));
#26207=CARTESIAN_POINT('Ctrl Pts',(17.2198652556304,0.0162647237884017,
4.5950091984451));
#26208=CARTESIAN_POINT('Ctrl Pts',(17.2211545887425,0.000283723793354941,
4.5949151055343));
#26209=CARTESIAN_POINT('Origin',(4.,0.,4.));
#26210=CARTESIAN_POINT('',(17.6288454112575,-0.000376811216598938,4.5933658344624));
#26211=CARTESIAN_POINT('',(17.5211545887425,0.000390292690419375,4.59338796628294));
#26212=CARTESIAN_POINT('',(4.,-7.27562663373442E-17,4.5941));
#26213=CARTESIAN_POINT('Ctrl Pts',(17.6288454112575,-0.000376811216598938,
4.5933658344624));
#26214=CARTESIAN_POINT('Ctrl Pts',(17.6188882305552,0.123868145157646,4.5926473455414));
#26215=CARTESIAN_POINT('Ctrl Pts',(17.608931049853,0.248515939035854,4.55458993700248));
#26216=CARTESIAN_POINT('Ctrl Pts',(17.5989738691507,0.348483110949462,4.48236965854082));
#26217=CARTESIAN_POINT('Ctrl Pts',(17.5830685904631,0.508167440925656,4.36700731952407));
#26218=CARTESIAN_POINT('Ctrl Pts',(17.5671633117754,0.604877102606476,4.16447556457896));
#26219=CARTESIAN_POINT('Ctrl Pts',(17.5512580330878,0.594207110796467,3.96776840716434));
#26220=CARTESIAN_POINT('Ctrl Pts',(17.5353527544002,0.583537118986457,3.77106124974973));
#26221=CARTESIAN_POINT('Ctrl Pts',(17.5194474757126,0.465487473685617,3.58017868986561));
#26222=CARTESIAN_POINT('Ctrl Pts',(17.503542197025,0.294261577747463,3.48276592343564));
#26223=CARTESIAN_POINT('Ctrl Pts',(17.4876369183374,0.123035681809298,3.38535315700567));
#26224=CARTESIAN_POINT('Ctrl Pts',(17.4717316396498,-0.101366464766187,
3.38141018402985));
#26225=CARTESIAN_POINT('Ctrl Pts',(17.4558263609621,-0.275908889943427,
3.47274745088526));
#26226=CARTESIAN_POINT('Ctrl Pts',(17.4399210822745,-0.450451315120656,
3.56408471774066));
#26227=CARTESIAN_POINT('Ctrl Pts',(17.4240158035869,-0.575134018899647,
3.75070222442727));
#26228=CARTESIAN_POINT('Ctrl Pts',(17.4081105248993,-0.592707978595278,
3.94691310701022));
#26229=CARTESIAN_POINT('Ctrl Pts',(17.3922052462117,-0.610281938290908,
4.14312398959316));
#26230=CARTESIAN_POINT('Ctrl Pts',(17.3762999675241,-0.520747153903178,
4.34892824807245));
#26231=CARTESIAN_POINT('Ctrl Pts',(17.3603946888365,-0.365214210518585,
4.46982927381454));
#26232=CARTESIAN_POINT('Ctrl Pts',(17.3498782629768,-0.262377240481122,
4.54976793433994));
#26233=CARTESIAN_POINT('Ctrl Pts',(17.3393618371172,-0.130687628661636,
4.59258915708319));
#26234=CARTESIAN_POINT('Ctrl Pts',(17.3288454112575,0.000452601584348983,
4.59351524744837));
#26235=CARTESIAN_POINT('Ctrl Pts',(17.2211545887425,0.000283723793354941,
4.5949151055343));
#26236=CARTESIAN_POINT('Ctrl Pts',(17.235770534318,-0.18087770297476,4.59384846352355));
#26237=CARTESIAN_POINT('Ctrl Pts',(17.2503864798935,-0.362942684182573,
4.50513801271133));
#26238=CARTESIAN_POINT('Ctrl Pts',(17.265002425469,-0.47285052735612,4.36129398677095));
#26239=CARTESIAN_POINT('Ctrl Pts',(17.2809077041566,-0.592453796716944,
4.20476088336606));
#26240=CARTESIAN_POINT('Ctrl Pts',(17.2968129828442,-0.626607860139456,
3.98293804780737));
#26241=CARTESIAN_POINT('Ctrl Pts',(17.3127182615318,-0.559630616639302,
3.79767714163318));
#26242=CARTESIAN_POINT('Ctrl Pts',(17.3286235402194,-0.492653373139145,
3.61241623545897));
#26243=CARTESIAN_POINT('Ctrl Pts',(17.3445288189071,-0.324544822716309,
3.46371725866926));
#26244=CARTESIAN_POINT('Ctrl Pts',(17.3604340975947,-0.132493299638714,
3.41985649047097));
#26245=CARTESIAN_POINT('Ctrl Pts',(17.3763393762823,0.0595582234388708,
3.37599572227269));
#26246=CARTESIAN_POINT('Ctrl Pts',(17.3922446549699,0.275552719171213,3.43697316266583));
#26247=CARTESIAN_POINT('Ctrl Pts',(17.4081499336575,0.416314653091553,3.5747905507646));
#26248=CARTESIAN_POINT('Ctrl Pts',(17.4240552123451,0.557076587011893,3.71260793886338));
#26249=CARTESIAN_POINT('Ctrl Pts',(17.4399604910327,0.622605959120231,3.92726527466781));
#26250=CARTESIAN_POINT('Ctrl Pts',(17.4558657697203,0.582814454063527,4.12020099097945));
#26251=CARTESIAN_POINT('Ctrl Pts',(17.4717710484079,0.543022949006823,4.31313670729109));
#26252=CARTESIAN_POINT('Ctrl Pts',(17.4876763270955,0.397910566785078,4.48435080410994));
#26253=CARTESIAN_POINT('Ctrl Pts',(17.5035816057832,0.214106774115907,4.55522901164789));
#26254=CARTESIAN_POINT('Ctrl Pts',(17.5094392667696,0.146414762764002,4.58133232736073));
#26255=CARTESIAN_POINT('Ctrl Pts',(17.515296927756,0.073474912906076,4.59382676872096));
#26256=CARTESIAN_POINT('Ctrl Pts',(17.5211545887425,0.000390292690419375,
4.59338796628294));
#26257=CARTESIAN_POINT('Origin',(4.,0.,4.));
#26258=CARTESIAN_POINT('',(17.9288454112575,-0.000301159635511528,4.59489313984584));
#26259=CARTESIAN_POINT('',(17.8211545887425,-0.000441626631060947,4.59348913571676));
#26260=CARTESIAN_POINT('',(4.,-7.27562663373442E-17,4.5941));
#26261=CARTESIAN_POINT('Ctrl Pts',(17.9288454112575,-0.000301159635511528,
4.59489313984584));
#26262=CARTESIAN_POINT('Ctrl Pts',(17.9143199026809,0.179756887528332,4.59377956832623));
#26263=CARTESIAN_POINT('Ctrl Pts',(17.8997943941043,0.360751589755073,4.50630604003092));
#26264=CARTESIAN_POINT('Ctrl Pts',(17.8852688855277,0.470789914960854,4.36397502945801));
#26265=CARTESIAN_POINT('Ctrl Pts',(17.8693636068401,0.591280720462369,4.20812407407766));
#26266=CARTESIAN_POINT('Ctrl Pts',(17.8534583281524,0.626694694978596,3.98649889312445));
#26267=CARTESIAN_POINT('Ctrl Pts',(17.8375530494648,0.560771239653389,3.80086039350393));
#26268=CARTESIAN_POINT('Ctrl Pts',(17.8216477707772,0.494847784328189,3.61522189388343));
#26269=CARTESIAN_POINT('Ctrl Pts',(17.8057424920896,0.327586899161578,3.46557007559562));
#26270=CARTESIAN_POINT('Ctrl Pts',(17.789837213402,0.135787706397568,3.42061872235194));
#26271=CARTESIAN_POINT('Ctrl Pts',(17.7739319347144,-0.0560114863664412,
3.37566736910827));
#26272=CARTESIAN_POINT('Ctrl Pts',(17.7580266560268,-0.272348986727849,
3.43541648090873));
#26273=CARTESIAN_POINT('Ctrl Pts',(17.7421213773392,-0.41389176700556,3.57243179339102));
#26274=CARTESIAN_POINT('Ctrl Pts',(17.7262160986515,-0.555434547283271,
3.7094471058733));
#26275=CARTESIAN_POINT('Ctrl Pts',(17.710310819964,-0.622182607477285,3.92372861903742));
#26276=CARTESIAN_POINT('Ctrl Pts',(17.6944055412763,-0.583488062224059,
4.11688732754162));
#26277=CARTESIAN_POINT('Ctrl Pts',(17.6785002625887,-0.544793516970831,
4.31004603604583));
#26278=CARTESIAN_POINT('Ctrl Pts',(17.6625949839011,-0.400656366270352,
4.48208193989012));
#26279=CARTESIAN_POINT('Ctrl Pts',(17.6466897052135,-0.217258291784321,
4.55400343026805));
#26280=CARTESIAN_POINT('Ctrl Pts',(17.6407416072282,-0.148672903323923,
4.58089991415997));
#26281=CARTESIAN_POINT('Ctrl Pts',(17.6347935092429,-0.0745967331795002,
4.59379503652584));
#26282=CARTESIAN_POINT('Ctrl Pts',(17.6288454112575,-0.000376811216598938,
4.5933658344624));
#26283=CARTESIAN_POINT('Ctrl Pts',(17.5211545887425,0.000390292690419375,
4.59338796628294));
#26284=CARTESIAN_POINT('Ctrl Pts',(17.5312022064437,-0.12497140465997,4.59263529057266));
#26285=CARTESIAN_POINT('Ctrl Pts',(17.5412498241448,-0.250759050797478,
4.55382993891589));
#26286=CARTESIAN_POINT('Ctrl Pts',(17.551297441846,-0.351218450958555,4.48038168762358));
#26287=CARTESIAN_POINT('Ctrl Pts',(17.5672027205336,-0.510244680247213,
4.36411383780432));
#26288=CARTESIAN_POINT('Ctrl Pts',(17.5831079992212,-0.605801935707933,
4.16103581990878));
#26289=CARTESIAN_POINT('Ctrl Pts',(17.5990132779088,-0.594014368327242,
3.96439246823218));
#26290=CARTESIAN_POINT('Ctrl Pts',(17.6149185565964,-0.58222680094655,3.76774911655557));
#26291=CARTESIAN_POINT('Ctrl Pts',(17.6308238352841,-0.463094410724447,
3.5775404310979));
#26292=CARTESIAN_POINT('Ctrl Pts',(17.6467291139717,-0.291317751175132,
3.48110219315546));
#26293=CARTESIAN_POINT('Ctrl Pts',(17.6626343926593,-0.119541091625818,
3.38466395521302));
#26294=CARTESIAN_POINT('Ctrl Pts',(17.6785396713469,0.104879837250709,3.38199616478582));
#26295=CARTESIAN_POINT('Ctrl Pts',(17.6944449500345,0.278900439380867,3.47432375837312));
#26296=CARTESIAN_POINT('Ctrl Pts',(17.7103502287221,0.452921041511034,3.56665135196042));
#26297=CARTESIAN_POINT('Ctrl Pts',(17.7262555074097,0.576541316894826,3.75397432956222));
#26298=CARTESIAN_POINT('Ctrl Pts',(17.7421607860974,0.593000065018554,3.95028190484542));
#26299=CARTESIAN_POINT('Ctrl Pts',(17.758066064785,0.60945881314228,4.1465894801286));
#26300=CARTESIAN_POINT('Ctrl Pts',(17.7739713434726,0.518756034005955,4.35188165309317));
#26301=CARTESIAN_POINT('Ctrl Pts',(17.7898766221602,0.362538606470845,4.47189694310939));
#26302=CARTESIAN_POINT('Ctrl Pts',(17.8003026110209,0.260137309937395,4.55056755941266));
#26303=CARTESIAN_POINT('Ctrl Pts',(17.8107285998817,0.129585238016204,4.59259583028147));
#26304=CARTESIAN_POINT('Ctrl Pts',(17.8211545887425,-0.000441626631060947,
4.59348913571676));
#26305=CARTESIAN_POINT('Origin',(4.,0.,4.));
#26306=CARTESIAN_POINT('',(18.2288454112575,0.000530626821107938,4.59429426521737));
#26307=CARTESIAN_POINT('',(18.1211545887425,-0.000206261771334874,4.59499421029555));
#26308=CARTESIAN_POINT('',(4.,-7.27562663373442E-17,4.5941));
#26309=CARTESIAN_POINT('Ctrl Pts',(18.2288454112575,0.000530626821107938,
4.59429426521737));
#26310=CARTESIAN_POINT('Ctrl Pts',(18.2256568534942,0.0401596894680921,
4.59466101186164));
#26311=CARTESIAN_POINT('Ctrl Pts',(18.2224682957309,0.0797220295111884,
4.5910372210354));
#26312=CARTESIAN_POINT('Ctrl Pts',(18.2192797379675,0.118424305077702,4.58317806034235));
#26313=CARTESIAN_POINT('Ctrl Pts',(18.2033744592799,0.311480390123117,4.54397471188459));
#26314=CARTESIAN_POINT('Ctrl Pts',(18.1874691805923,0.483135922039688,4.39938477867344));
#26315=CARTESIAN_POINT('Ctrl Pts',(18.1715639019047,0.554573942717995,4.21579784094385));
#26316=CARTESIAN_POINT('Ctrl Pts',(18.1556586232171,0.626011963396302,4.03221090321426));
#26317=CARTESIAN_POINT('Ctrl Pts',(18.1397533445295,0.597232472836345,3.80962696096622));
#26318=CARTESIAN_POINT('Ctrl Pts',(18.1238480658419,0.481449795543417,3.65024714373002));
#26319=CARTESIAN_POINT('Ctrl Pts',(18.1079427871543,0.365667118250483,3.49086732649381));
#26320=CARTESIAN_POINT('Ctrl Pts',(18.0920375084667,0.16288125422457,3.39469163426944));
#26321=CARTESIAN_POINT('Ctrl Pts',(18.076132229779,-0.0337971069360236,
3.40587987606835));
#26322=CARTESIAN_POINT('Ctrl Pts',(18.0602269510914,-0.230475468096606,
3.41706811786726));
#26323=CARTESIAN_POINT('Ctrl Pts',(18.0443216724038,-0.421046326391869,
3.53562029368944));
#26324=CARTESIAN_POINT('Ctrl Pts',(18.0284163937162,-0.518007606080761,
3.70710225992629));
#26325=CARTESIAN_POINT('Ctrl Pts',(18.0125111150286,-0.614968885769652,
3.87858422616314));
#26326=CARTESIAN_POINT('Ctrl Pts',(17.996605836341,-0.618320586852172,4.10299598281466));
#26327=CARTESIAN_POINT('Ctrl Pts',(17.9807005576534,-0.526523749990007,
4.27729714530494));
#26328=CARTESIAN_POINT('Ctrl Pts',(17.9647952789658,-0.434726913127837,
4.45159830779523));
#26329=CARTESIAN_POINT('Ctrl Pts',(17.9488900002781,-0.247781538320971,
4.57578887612429));
#26330=CARTESIAN_POINT('Ctrl Pts',(17.9329847215905,-0.0515250326741526,
4.59284579538505));
#26331=CARTESIAN_POINT('Ctrl Pts',(17.9316049514795,-0.0344999389365885,
4.59432546938787));
#26332=CARTESIAN_POINT('Ctrl Pts',(17.9302251813685,-0.0174047750035579,
4.59499891739512));
#26333=CARTESIAN_POINT('Ctrl Pts',(17.9288454112575,-0.000301159635511528,
4.59489313984584));
#26334=CARTESIAN_POINT('Ctrl Pts',(17.8211545887425,-0.000441626631060947,
4.59348913571676));
#26335=CARTESIAN_POINT('Ctrl Pts',(17.8266338785693,-0.0687761401428734,
4.59395860479535));
#26336=CARTESIAN_POINT('Ctrl Pts',(17.8321131683962,-0.136965594625977,
4.58306684864343));
#26337=CARTESIAN_POINT('Ctrl Pts',(17.837592458223,-0.200847632772524,4.56016175744822));
#26338=CARTESIAN_POINT('Ctrl Pts',(17.8534977369106,-0.386284368546891,
4.49367287470298));
#26339=CARTESIAN_POINT('Ctrl Pts',(17.8694030155983,-0.535425764161732,
4.32595670214462));
#26340=CARTESIAN_POINT('Ctrl Pts',(17.8853082942859,-0.579792400402821,
4.13402141072584));
#26341=CARTESIAN_POINT('Ctrl Pts',(17.9012135729735,-0.624159036643913,
3.94208611930704));
#26342=CARTESIAN_POINT('Ctrl Pts',(17.9171188516611,-0.563750913511241,
3.72593170902781));
#26343=CARTESIAN_POINT('Ctrl Pts',(17.9330241303487,-0.426304885490399,
3.58480714034942));
#26344=CARTESIAN_POINT('Ctrl Pts',(17.9489294090363,-0.288858857469565,
3.44368257167104));
#26345=CARTESIAN_POINT('Ctrl Pts',(17.9648346877239,-0.0743749245605683,
3.37758784459349));
#26346=CARTESIAN_POINT('Ctrl Pts',(17.9807399664116,0.118664965311668,3.41687086155347));
#26347=CARTESIAN_POINT('Ctrl Pts',(17.9966452450992,0.311704855183904,3.45615387851346));
#26348=CARTESIAN_POINT('Ctrl Pts',(18.0125505237868,0.483300702019379,3.60081463951098));
#26349=CARTESIAN_POINT('Ctrl Pts',(18.0284558024744,0.554662952572844,3.78443104318807));
#26350=CARTESIAN_POINT('Ctrl Pts',(18.044361081162,0.62602520312631,3.96804744686516));
#26351=CARTESIAN_POINT('Ctrl Pts',(18.0602663598496,0.597153857397765,4.19061949322182));
#26352=CARTESIAN_POINT('Ctrl Pts',(18.0761716385372,0.481305415899848,4.34995151481781));
#26353=CARTESIAN_POINT('Ctrl Pts',(18.0911659552723,0.372092100044007,4.50015792394613));
#26354=CARTESIAN_POINT('Ctrl Pts',(18.1061602720074,0.185579460002099,4.59416090236354));
#26355=CARTESIAN_POINT('Ctrl Pts',(18.1211545887425,-0.000206261771334874,
4.59499421029555));
#26356=CARTESIAN_POINT('Origin',(4.,0.,4.));
#26357=CARTESIAN_POINT('',(18.5288454112575,4.04073003155148E-5,4.59311858068669));
#26358=CARTESIAN_POINT('',(18.4211545887425,0.000547083855738422,4.59411609730493));
#26359=CARTESIAN_POINT('',(4.,-7.27562663373442E-17,4.5941));
#26360=CARTESIAN_POINT('Ctrl Pts',(18.5288454112575,4.04073003155148E-5,
4.59311858068669));
#26361=CARTESIAN_POINT('Ctrl Pts',(18.5210885256199,0.0969311390001333,
4.59317716754242));
#26362=CARTESIAN_POINT('Ctrl Pts',(18.5133316399822,0.193796352446061,4.57078374547556));
#26363=CARTESIAN_POINT('Ctrl Pts',(18.5055747543446,0.27868347559656,4.52579129559858));
#26364=CARTESIAN_POINT('Ctrl Pts',(18.489669475657,0.452742165355285,4.43353552600749));
#26365=CARTESIAN_POINT('Ctrl Pts',(18.4737641969693,0.576439736070726,4.24626358090446));
#26366=CARTESIAN_POINT('Ctrl Pts',(18.4578589182817,0.592979496483005,4.04996281465819));
#26367=CARTESIAN_POINT('Ctrl Pts',(18.4419536395941,0.609519256895283,3.85366204841193));
#26368=CARTESIAN_POINT('Ctrl Pts',(18.4260483609065,0.518901207004412,3.64833246102244));
#26369=CARTESIAN_POINT('Ctrl Pts',(18.4101430822189,0.362733321586741,3.52825271224048));
#26370=CARTESIAN_POINT('Ctrl Pts',(18.3942378035313,0.206565436169079,3.40817296345854));
#26371=CARTESIAN_POINT('Ctrl Pts',(18.3783325248437,-0.015152284775374,
3.37334305328413));
#26372=CARTESIAN_POINT('Ctrl Pts',(18.3624272461561,-0.200616443892158,
3.43975540293737));
#26373=CARTESIAN_POINT('Ctrl Pts',(18.3465219674685,-0.386080603008964,
3.50616775259061));
#26374=CARTESIAN_POINT('Ctrl Pts',(18.3306166887808,-0.535291200298091,
3.67382236207151));
#26375=CARTESIAN_POINT('Ctrl Pts',(18.3147114100932,-0.579737042064157,
3.86573932758804));
#26376=CARTESIAN_POINT('Ctrl Pts',(18.2988061314056,-0.624182883830224,
4.05765629310458));
#26377=CARTESIAN_POINT('Ctrl Pts',(18.282900852718,-0.563863970073232,4.27383561465674));
#26378=CARTESIAN_POINT('Ctrl Pts',(18.2669955740304,-0.426476194107598,
4.41501689358062));
#26379=CARTESIAN_POINT('Ctrl Pts',(18.2542788531061,-0.316630774880643,
4.52789532589669));
#26380=CARTESIAN_POINT('Ctrl Pts',(18.2415621321818,-0.157519428275204,
4.5928315930404));
#26381=CARTESIAN_POINT('Ctrl Pts',(18.2288454112575,0.000530626821107938,
4.59429426521737));
#26382=CARTESIAN_POINT('Ctrl Pts',(18.1211545887425,-0.000206261771334874,
4.59499421029555));
#26383=CARTESIAN_POINT('Ctrl Pts',(18.122065550695,-0.0114934532352288,
4.59504483693191));
#26384=CARTESIAN_POINT('Ctrl Pts',(18.1229765126475,-0.0227779616248223,
4.59475157188293));
#26385=CARTESIAN_POINT('Ctrl Pts',(18.1238874746001,-0.0340422900297544,
4.59410612569417));
#26386=CARTESIAN_POINT('Ctrl Pts',(18.1397927532877,-0.230716017194119,
4.58283671813918));
#26387=CARTESIAN_POINT('Ctrl Pts',(18.1556980319753,-0.421237934255556,
4.46420590619388));
#26388=CARTESIAN_POINT('Ctrl Pts',(18.1716033106629,-0.518128437217054,
4.29268393984778));
#26389=CARTESIAN_POINT('Ctrl Pts',(18.1875085893505,-0.615018940178556,
4.12116197350168));
#26390=CARTESIAN_POINT('Ctrl Pts',(18.2034138680381,-0.618278029040109,
3.89674885275477));
#26391=CARTESIAN_POINT('Ctrl Pts',(18.2193191467258,-0.526409268077163,
3.72248558851787));
#26392=CARTESIAN_POINT('Ctrl Pts',(18.2352244254134,-0.434540507114227,
3.54822232428098));
#26393=CARTESIAN_POINT('Ctrl Pts',(18.251129704101,-0.24754389632682,3.42410891655409));
#26394=CARTESIAN_POINT('Ctrl Pts',(18.2670349827886,-0.0512803682143169,
3.40713299136011));
#26395=CARTESIAN_POINT('Ctrl Pts',(18.2829402614762,0.144983159898198,3.39015706616613));
#26396=CARTESIAN_POINT('Ctrl Pts',(18.2988455401638,0.35051360533581,3.48031862350507));
#26397=CARTESIAN_POINT('Ctrl Pts',(18.3147508188514,0.470940082829639,3.63621929066782));
#26398=CARTESIAN_POINT('Ctrl Pts',(18.330656097539,0.591366560323475,3.79211995783059));
#26399=CARTESIAN_POINT('Ctrl Pts',(18.3465613762266,0.62668906987352,4.01375973481717));
#26400=CARTESIAN_POINT('Ctrl Pts',(18.3624666549143,0.560689009466533,4.199371012841));
#26401=CARTESIAN_POINT('Ctrl Pts',(18.3783719336019,0.49468894905955,4.38498229086483));
#26402=CARTESIAN_POINT('Ctrl Pts',(18.3942772122895,0.327366318695548,4.53456506992591));
#26403=CARTESIAN_POINT('Ctrl Pts',(18.4101824909771,0.135548591400956,4.57943726620491));
#26404=CARTESIAN_POINT('Ctrl Pts',(18.4138398568989,0.0914407431336166,
4.58975547846199));
#26405=CARTESIAN_POINT('Ctrl Pts',(18.4174972228207,0.0460377050408626,
4.59453706917327));
#26406=CARTESIAN_POINT('Ctrl Pts',(18.4211545887425,0.000547083855738422,
4.59411609730493));
#26407=CARTESIAN_POINT('Origin',(4.,0.,4.));
#26408=CARTESIAN_POINT('',(18.8288454112575,-0.000545657836941327,4.59414547262434));
#26409=CARTESIAN_POINT('',(18.7211545887425,-5.63168744233308E-5,4.59312091231189));
#26410=CARTESIAN_POINT('',(4.,-7.27562663373442E-17,4.5941));
#26411=CARTESIAN_POINT('Ctrl Pts',(18.8288454112575,-0.000545657836941327,
4.59414547262434));
#26412=CARTESIAN_POINT('Ctrl Pts',(18.8165201977456,0.15273698101805,4.59272393327212));
#26413=CARTESIAN_POINT('Ctrl Pts',(18.8041949842336,0.307016766534516,4.53213273669464));
#26414=CARTESIAN_POINT('Ctrl Pts',(18.7918697707216,0.416139138999065,4.42538122089617));
#26415=CARTESIAN_POINT('Ctrl Pts',(18.775964492034,0.556957936451544,4.28762193522949));
#26416=CARTESIAN_POINT('Ctrl Pts',(18.7600592133464,0.622575889387102,4.0729916608594));
#26417=CARTESIAN_POINT('Ctrl Pts',(18.7441539346588,0.582864009884755,3.88003953951897));
#26418=CARTESIAN_POINT('Ctrl Pts',(18.7282486559712,0.543152130382401,3.6870874181785));
#26419=CARTESIAN_POINT('Ctrl Pts',(18.7123433772835,0.3981104184421,3.51581344986768));
#26420=CARTESIAN_POINT('Ctrl Pts',(18.6964380985959,0.214335891977863,3.44485939483061));
#26421=CARTESIAN_POINT('Ctrl Pts',(18.6805328199083,0.0305613655136472,
3.37390533979354));
#26422=CARTESIAN_POINT('Ctrl Pts',(18.6646275412207,-0.191945975474496,
3.40327119803019));
#26423=CARTESIAN_POINT('Ctrl Pts',(18.6487222625331,-0.351020173514001,
3.51947340980541));
#26424=CARTESIAN_POINT('Ctrl Pts',(18.6328169838455,-0.510094371553506,
3.63567562158063));
#26425=CARTESIAN_POINT('Ctrl Pts',(18.6169117051579,-0.605735426644373,
3.83871418689441));
#26426=CARTESIAN_POINT('Ctrl Pts',(18.6010064264702,-0.594029012528289,
4.03536238640794));
#26427=CARTESIAN_POINT('Ctrl Pts',(18.5851011477826,-0.582322598412206,
4.23201058592146));
#26428=CARTESIAN_POINT('Ctrl Pts',(18.569195869095,-0.463268715089173,4.42226841963472));
#26429=CARTESIAN_POINT('Ctrl Pts',(18.5532905904074,-0.29153186902666,4.51877753945177));
#26430=CARTESIAN_POINT('Ctrl Pts',(18.5451421973574,-0.203549800283198,
4.56821988225003));
#26431=CARTESIAN_POINT('Ctrl Pts',(18.5369938043075,-0.101740616897797,
4.59305703682098));
#26432=CARTESIAN_POINT('Ctrl Pts',(18.5288454112575,4.04073003155148E-5,
4.59311858068669));
#26433=CARTESIAN_POINT('Ctrl Pts',(18.4211545887425,0.000547083855738422,
4.59411609730493));
#26434=CARTESIAN_POINT('Ctrl Pts',(18.4334025015083,-0.151793472668411,
4.59270633223614));
#26435=CARTESIAN_POINT('Ctrl Pts',(18.4456504142741,-0.305116246576315,
4.53295143150856));
#26436=CARTESIAN_POINT('Ctrl Pts',(18.4578983270399,-0.414068183831284,
4.42739736222451));
#26437=CARTESIAN_POINT('Ctrl Pts',(18.4738036057275,-0.555554407543751,
4.29032364846819));
#26438=CARTESIAN_POINT('Ctrl Pts',(18.4897088844152,-0.622214030743504,
4.07601460745865));
#26439=CARTESIAN_POINT('Ctrl Pts',(18.5056141631028,-0.583439774593308,
3.88287188415962));
#26440=CARTESIAN_POINT('Ctrl Pts',(18.5215194417904,-0.54466551844311,3.68972916086059));
#26441=CARTESIAN_POINT('Ctrl Pts',(18.537424720478,-0.400457382942952,3.51775275527208));
#26442=CARTESIAN_POINT('Ctrl Pts',(18.5533299991656,-0.217029642971419,
3.44590695711865));
#26443=CARTESIAN_POINT('Ctrl Pts',(18.5692352778532,-0.0336019029998957,
3.37406115896522));
#26444=CARTESIAN_POINT('Ctrl Pts',(18.5851405565408,0.189045441442997,3.40234596824686));
#26445=CARTESIAN_POINT('Ctrl Pts',(18.6010458352284,0.348682149221421,3.51777419717301));
#26446=CARTESIAN_POINT('Ctrl Pts',(18.6169511139161,0.508318856999844,3.63320242609916));
#26447=CARTESIAN_POINT('Ctrl Pts',(18.6328563926037,0.604944928113798,3.83577407466982));
#26448=CARTESIAN_POINT('Ctrl Pts',(18.6487616712913,0.594193758619731,4.03247681196108));
#26449=CARTESIAN_POINT('Ctrl Pts',(18.6646669499789,0.583442589125664,4.22917954925235));
#26450=CARTESIAN_POINT('Ctrl Pts',(18.6805722286665,0.465314179023576,4.42001337526422));
#26451=CARTESIAN_POINT('Ctrl Pts',(18.6964775073541,0.294048096631404,4.51735547060535));
#26452=CARTESIAN_POINT('Ctrl Pts',(18.7047032011502,0.205474838715737,4.56769764225005));
#26453=CARTESIAN_POINT('Ctrl Pts',(18.7129288949463,0.102689258835563,4.59303430424318));
#26454=CARTESIAN_POINT('Ctrl Pts',(18.7211545887425,-5.63168744233308E-5,
4.59312091231189));
#26455=CARTESIAN_POINT('Origin',(4.,0.,4.));
#26456=CARTESIAN_POINT('',(19.1288454112575,0.000222628893785728,4.59497983522242));
#26457=CARTESIAN_POINT('',(19.0211545887425,-0.000526118841417405,4.59432346427954));
#26458=CARTESIAN_POINT('',(4.,-7.27562663373442E-17,4.5941));
#26459=CARTESIAN_POINT('Ctrl Pts',(19.1288454112575,0.000222628893785728,
4.59497983522242));
#26460=CARTESIAN_POINT('Ctrl Pts',(19.1278571485589,0.012468395078646,4.59503853204781));
#26461=CARTESIAN_POINT('Ctrl Pts',(19.1268688858602,0.0247107891953784,
4.59469333777414));
#26462=CARTESIAN_POINT('Ctrl Pts',(19.1258806231615,0.0369274203756033,
4.59393377720877));
#26463=CARTESIAN_POINT('Ctrl Pts',(19.1099753444739,0.233544093050454,4.58170927203582));
#26464=CARTESIAN_POINT('Ctrl Pts',(19.0940700657862,0.423487581379576,4.46215450773496));
#26465=CARTESIAN_POINT('Ctrl Pts',(19.0781647870986,0.519543871337238,4.29016397409385));
#26466=CARTESIAN_POINT('Ctrl Pts',(19.062259508411,0.615600161294901,4.11817344045274));
#26467=CARTESIAN_POINT('Ctrl Pts',(19.0463542297234,0.617769252881104,3.89374713747137));
#26468=CARTESIAN_POINT('Ctrl Pts',(19.0304489510358,0.525055191022736,3.71993212880311));
#26469=CARTESIAN_POINT('Ctrl Pts',(19.0145436723482,0.432341129164367,3.54611712013485));
#26470=CARTESIAN_POINT('Ctrl Pts',(18.9986383936606,0.244743913861428,3.42291340577968));
#26471=CARTESIAN_POINT('Ctrl Pts',(18.982733114973,0.0484002497885746,3.40689091904056));
#26472=CARTESIAN_POINT('Ctrl Pts',(18.9668278362853,-0.147943414284278,
3.39086843230144));
#26473=CARTESIAN_POINT('Ctrl Pts',(18.9509225575977,-0.353033527127044,
3.48202717317836));
#26474=CARTESIAN_POINT('Ctrl Pts',(18.9350172789101,-0.472701385564812,
3.63851090447403));
#26475=CARTESIAN_POINT('Ctrl Pts',(18.9191120002225,-0.592369244002587,
3.79499463576972));
#26476=CARTESIAN_POINT('Ctrl Pts',(18.9032067215349,-0.626614848035354,
4.01680335748416));
#26477=CARTESIAN_POINT('Ctrl Pts',(18.8873014428473,-0.559714065105754,
4.20209188855652));
#26478=CARTESIAN_POINT('Ctrl Pts',(18.8713961641597,-0.492813282176159,
4.38738041962887));
#26479=CARTESIAN_POINT('Ctrl Pts',(18.8554908854721,-0.324766112284209,
4.53614876005914));
#26480=CARTESIAN_POINT('Ctrl Pts',(18.8395856067844,-0.132732706353525,
4.58008878179264));
#26481=CARTESIAN_POINT('Ctrl Pts',(18.8360055416088,-0.0895085590353085,
4.5899790920924));
#26482=CARTESIAN_POINT('Ctrl Pts',(18.8324254764332,-0.0450691735440342,
4.59455838259347));
#26483=CARTESIAN_POINT('Ctrl Pts',(18.8288454112575,-0.000545657836941327,
4.59414547262434));
#26484=CARTESIAN_POINT('Ctrl Pts',(18.7211545887425,-5.63168744233308E-5,
4.59312091231189));
#26485=CARTESIAN_POINT('Ctrl Pts',(18.728834173634,-0.0959805501911411,
4.59320177041728));
#26486=CARTESIAN_POINT('Ctrl Pts',(18.7365137585255,-0.191869914813978,
4.57127401300463));
#26487=CARTESIAN_POINT('Ctrl Pts',(18.744193343417,-0.276126457005151,4.5271386400555));
#26488=CARTESIAN_POINT('Ctrl Pts',(18.7600986221046,-0.450631173567243,
4.43572934949413));
#26489=CARTESIAN_POINT('Ctrl Pts',(18.7760039007922,-0.575236852009173,
4.249060403701));
#26490=CARTESIAN_POINT('Ctrl Pts',(18.7919091794798,-0.592729836422094,
4.05284228527226));
#26491=CARTESIAN_POINT('Ctrl Pts',(18.8078144581674,-0.610222820835014,
3.85662416684351));
#26492=CARTESIAN_POINT('Ctrl Pts',(18.823719736855,-0.520603111218926,3.65085687577915));
#26493=CARTESIAN_POINT('Ctrl Pts',(18.8396250155426,-0.365020286731977,
3.53002004684018));
#26494=CARTESIAN_POINT('Ctrl Pts',(18.8555302942302,-0.209437462245028,
3.40918321790122));
#26495=CARTESIAN_POINT('Ctrl Pts',(18.8714355729179,0.0121084771127808,
3.37327685108765));
#26496=CARTESIAN_POINT('Ctrl Pts',(18.8873408516055,0.197893008823487,3.43878763096633));
#26497=CARTESIAN_POINT('Ctrl Pts',(18.9032461302931,0.383677540534204,3.50429841084501));
#26498=CARTESIAN_POINT('Ctrl Pts',(18.9191514089807,0.533700664597814,3.67122633741595));
#26499=CARTESIAN_POINT('Ctrl Pts',(18.9350566876683,0.579078109400399,3.86292516893752));
#26500=CARTESIAN_POINT('Ctrl Pts',(18.9509619663559,0.624455554202981,4.05462400045908));
#26501=CARTESIAN_POINT('Ctrl Pts',(18.9668672450435,0.56518731974455,4.27109373693126));
#26502=CARTESIAN_POINT('Ctrl Pts',(18.9827725237311,0.428486871854059,4.41294063344238));
#26503=CARTESIAN_POINT('Ctrl Pts',(18.9955665454016,0.318526617336051,4.52704063153052));
#26504=CARTESIAN_POINT('Ctrl Pts',(19.008360567072,0.158464569423419,4.5928566151945));
#26505=CARTESIAN_POINT('Ctrl Pts',(19.0211545887425,-0.000526118841417405,
4.59432346427954));
#26506=CARTESIAN_POINT('Origin',(4.,0.,4.));
#26507=CARTESIAN_POINT('',(19.4288454112575,0.000431836873498515,4.59346738712276));
#26508=CARTESIAN_POINT('',(19.3211545887425,0.000315695961457875,4.59487351203822));
#26509=CARTESIAN_POINT('',(4.,-7.27562663373442E-17,4.5941));
#26510=CARTESIAN_POINT('Ctrl Pts',(19.4288454112575,0.000431836873498515,
4.59346738712276));
#26511=CARTESIAN_POINT('Ctrl Pts',(19.4232888206845,0.0697367837969298,
4.59393182999066));
#26512=CARTESIAN_POINT('Ctrl Pts',(19.4177322301115,0.13889623855249,4.58272225272434));
#26513=CARTESIAN_POINT('Ctrl Pts',(19.4121756395385,0.203565929825556,4.55917964700716));
#26514=CARTESIAN_POINT('Ctrl Pts',(19.3962703608509,0.38867754617092,4.49179089484985));
#26515=CARTESIAN_POINT('Ctrl Pts',(19.3803650821633,0.537002597765565,4.32335233206236));
#26516=CARTESIAN_POINT('Ctrl Pts',(19.3644598034757,0.580436494614329,4.13120381907284));
#26517=CARTESIAN_POINT('Ctrl Pts',(19.3485545247881,0.623870391463095,3.93905530608331));
#26518=CARTESIAN_POINT('Ctrl Pts',(19.3326492461004,0.562413133565966,3.72319684289176));
#26519=CARTESIAN_POINT('Ctrl Pts',(19.3167439674128,0.424283294458304,3.58274150440131));
#26520=CARTESIAN_POINT('Ctrl Pts',(19.3008386887252,0.286153455350651,3.44228616591086));
#26521=CARTESIAN_POINT('Ctrl Pts',(19.2849334100376,0.071351035032473,3.37723395212151));
#26522=CARTESIAN_POINT('Ctrl Pts',(19.26902813135,-0.12149578302492,3.4174540870367));
#26523=CARTESIAN_POINT('Ctrl Pts',(19.2531228526624,-0.314342601082313,
3.45767422195189));
#26524=CARTESIAN_POINT('Ctrl Pts',(19.2372175739748,-0.485233816878921,
3.60316670557164));
#26525=CARTESIAN_POINT('Ctrl Pts',(19.2213122952871,-0.555703413721375,
3.78712754492824));
#26526=CARTESIAN_POINT('Ctrl Pts',(19.2054070165995,-0.626173010563829,
3.97108838428485));
#26527=CARTESIAN_POINT('Ctrl Pts',(19.1895017379119,-0.59622098845213,4.19351757937831));
#26528=CARTESIAN_POINT('Ctrl Pts',(19.1735964592243,-0.479600048885993,
4.35228505390253));
#26529=CARTESIAN_POINT('Ctrl Pts',(19.1586794432354,-0.370225264934164,
4.50118762911129));
#26530=CARTESIAN_POINT('Ctrl Pts',(19.1437624272465,-0.184617181632464,
4.59409385471947));
#26531=CARTESIAN_POINT('Ctrl Pts',(19.1288454112575,0.000222628893785728,
4.59497983522242));
#26532=CARTESIAN_POINT('Ctrl Pts',(19.0211545887425,-0.000526118841417405,
4.59432346427954));
#26533=CARTESIAN_POINT('Ctrl Pts',(19.0242658457596,-0.0391895592568775,
4.59468017342281));
#26534=CARTESIAN_POINT('Ctrl Pts',(19.0273771027768,-0.0777896429211806,
4.59123148246997));
#26535=CARTESIAN_POINT('Ctrl Pts',(19.030488359794,-0.115590453236054,4.58374636034569));
#26536=CARTESIAN_POINT('Ctrl Pts',(19.0463936384816,-0.308834669113126,
4.5454811341878));
#26537=CARTESIAN_POINT('Ctrl Pts',(19.0622989171692,-0.481190439544719,
4.40172662532195));
#26538=CARTESIAN_POINT('Ctrl Pts',(19.0782041958568,-0.553519286527586,
4.21848882245705));
#26539=CARTESIAN_POINT('Ctrl Pts',(19.0941094745444,-0.625848133510457,
4.03525101959215));
#26540=CARTESIAN_POINT('Ctrl Pts',(19.1100147532321,-0.598150057044591,
3.81252992272818));
#26541=CARTESIAN_POINT('Ctrl Pts',(19.1259200319197,-0.483142842019737,
3.65258963701249));
#26542=CARTESIAN_POINT('Ctrl Pts',(19.1418253106073,-0.36813562699489,3.49264935129682));
#26543=CARTESIAN_POINT('Ctrl Pts',(19.1577305892949,-0.165819273411065,
3.39548987672941));
#26544=CARTESIAN_POINT('Ctrl Pts',(19.1736358679825,0.0309111084379188,
3.40572273351557));
#26545=CARTESIAN_POINT('Ctrl Pts',(19.1895411466701,0.227641490286902,3.41595559030173));
#26546=CARTESIAN_POINT('Ctrl Pts',(19.2054464253577,0.418785900401045,3.53358077844144));
#26547=CARTESIAN_POINT('Ctrl Pts',(19.2213517040453,0.516578912360374,3.70458978792342));
#26548=CARTESIAN_POINT('Ctrl Pts',(19.237256982733,0.614371924319703,3.87559879740541));
#26549=CARTESIAN_POINT('Ctrl Pts',(19.2531622614206,0.618813538124218,4.09999162822965));
#26550=CARTESIAN_POINT('Ctrl Pts',(19.2690675401082,0.527864352527146,4.27473658562515));
#26551=CARTESIAN_POINT('Ctrl Pts',(19.2849728187958,0.436915166930073,4.44948154302064));
#26552=CARTESIAN_POINT('Ctrl Pts',(19.3008780974834,0.250575181931413,4.5745786269874));
#26553=CARTESIAN_POINT('Ctrl Pts',(19.316783376171,0.0544038354309166,4.59258854924263));
#26554=CARTESIAN_POINT('Ctrl Pts',(19.3182404470282,0.0364327229714708,
4.59423842494573));
#26555=CARTESIAN_POINT('Ctrl Pts',(19.3196975178853,0.0183791031991185,
4.59498959766064));
#26556=CARTESIAN_POINT('Ctrl Pts',(19.3211545887425,0.000315695961457875,
4.59487351203822));
#26557=CARTESIAN_POINT('Origin',(4.,0.,4.));
#26558=CARTESIAN_POINT('',(19.7288454112575,-0.000401422265437046,4.59340756962635));
#26559=CARTESIAN_POINT('',(19.6211545887425,0.000364945106097663,4.59334757974602));
#26560=CARTESIAN_POINT('',(4.,-7.27562663373442E-17,4.5941));
#26561=CARTESIAN_POINT('Ctrl Pts',(19.7288454112575,-0.000401422265437046,
4.59340756962635));
#26562=CARTESIAN_POINT('Ctrl Pts',(19.7187204928102,0.125914276337785,4.59262579220321));
#26563=CARTESIAN_POINT('Ctrl Pts',(19.7085955743629,0.252675872983383,4.55317429478549));
#26564=CARTESIAN_POINT('Ctrl Pts',(19.6984706559155,0.353547469597214,4.47867015725961));
#26565=CARTESIAN_POINT('Ctrl Pts',(19.6825653772279,0.512007102052776,4.36163128164859));
#26566=CARTESIAN_POINT('Ctrl Pts',(19.6666600985403,0.606576931433326,4.15809158444534));
#26567=CARTESIAN_POINT('Ctrl Pts',(19.6507548198527,0.593834428727047,3.9615078130365));
#26568=CARTESIAN_POINT('Ctrl Pts',(19.6348495411651,0.581091926020768,3.76492404162769));
#26569=CARTESIAN_POINT('Ctrl Pts',(19.6189442624775,0.46103709122769,3.57529619601327));
#26570=CARTESIAN_POINT('Ctrl Pts',(19.6030389837899,0.288794059426421,3.47969339775167));
#26571=CARTESIAN_POINT('Ctrl Pts',(19.5871337051022,0.116551027625133,3.38409059949006));
#26572=CARTESIAN_POINT('Ctrl Pts',(19.5712284264146,-0.107880201184358,
3.38251284858128));
#26573=CARTESIAN_POINT('Ctrl Pts',(19.555323147727,-0.281450319664219,3.47568456171554));
#26574=CARTESIAN_POINT('Ctrl Pts',(19.5394178690394,-0.45502043814407,3.5688562748498));
#26575=CARTESIAN_POINT('Ctrl Pts',(19.5235125903518,-0.577729446294298,
3.75677745202708));
#26576=CARTESIAN_POINT('Ctrl Pts',(19.5076073116642,-0.593234549413986,
3.95316264945144));
#26577=CARTESIAN_POINT('Ctrl Pts',(19.4917020329766,-0.608739652533674,
4.1495478468758));
#26578=CARTESIAN_POINT('Ctrl Pts',(19.475796754289,-0.517040850622822,4.35439706454724));
#26579=CARTESIAN_POINT('Ctrl Pts',(19.4598914756013,-0.360242359119356,
4.47365220261941));
#26580=CARTESIAN_POINT('Ctrl Pts',(19.4495427874867,-0.258222223711561,
4.55124494740629));
#26581=CARTESIAN_POINT('Ctrl Pts',(19.4391940993721,-0.128642866595325,
4.59260240088276));
#26582=CARTESIAN_POINT('Ctrl Pts',(19.4288454112575,0.000431836873498515,
4.59346738712276));
#26583=CARTESIAN_POINT('Ctrl Pts',(19.3211545887425,0.000315695961457875,
4.59487351203822));
#26584=CARTESIAN_POINT('Ctrl Pts',(19.3356027965729,-0.178799726336078,
4.59372241551416));
#26585=CARTESIAN_POINT('Ctrl Pts',(19.3500510044034,-0.35887750705714,4.50729762043595));
#26586=CARTESIAN_POINT('Ctrl Pts',(19.3644992122339,-0.469016560662847,
4.36625733020606));
#26587=CARTESIAN_POINT('Ctrl Pts',(19.3804044909215,-0.590262902253753,
4.21099342837053));
#26588=CARTESIAN_POINT('Ctrl Pts',(19.3963097696091,-0.626752877433238,
3.98954286415574));
#26589=CARTESIAN_POINT('Ctrl Pts',(19.4122150482967,-0.561731832709929,
3.80358636875254));
#26590=CARTESIAN_POINT('Ctrl Pts',(19.4281203269843,-0.49671078798662,3.61762987334934));
#26591=CARTESIAN_POINT('Ctrl Pts',(19.4440256056719,-0.330178723360516,
3.46716744675772));
#26592=CARTESIAN_POINT('Ctrl Pts',(19.4599308843595,-0.138600118749324,
3.42128506802099));
#26593=CARTESIAN_POINT('Ctrl Pts',(19.4758361630471,0.0529784858618673,
3.37540268928427));
#26594=CARTESIAN_POINT('Ctrl Pts',(19.4917414417347,0.269603630458146,3.43410035840244));
#26595=CARTESIAN_POINT('Ctrl Pts',(19.5076467204224,0.411810215621333,3.57042659223364));
#26596=CARTESIAN_POINT('Ctrl Pts',(19.52355199911,0.554016800784528,3.70675282606484));
#26597=CARTESIAN_POINT('Ctrl Pts',(19.5394572777976,0.621804826514621,3.92070762460909));
#26598=CARTESIAN_POINT('Ctrl Pts',(19.5553625564852,0.584048894878601,4.11405198996909));
#26599=CARTESIAN_POINT('Ctrl Pts',(19.5712678351728,0.546292963242583,4.30739635532907));
#26600=CARTESIAN_POINT('Ctrl Pts',(19.5871731138604,0.402993074240464,4.4801302875048));
#26601=CARTESIAN_POINT('Ctrl Pts',(19.6030783925481,0.219946482677819,4.55294168410437));
#26602=CARTESIAN_POINT('Ctrl Pts',(19.6091037912795,0.150602919307179,4.5805248346624));
#26603=CARTESIAN_POINT('Ctrl Pts',(19.615129190011,0.0755552166468998,4.59376787586841));
#26604=CARTESIAN_POINT('Ctrl Pts',(19.6211545887425,0.000364945106097663,
4.59334757974602));
#26605=CARTESIAN_POINT('Origin',(4.,0.,4.));
#26606=CARTESIAN_POINT('',(20.0288454112575,-0.000266600559035268,4.5949350414008));
#26607=CARTESIAN_POINT('',(19.9211545887425,-0.000461335262921832,4.59353843444423));
#26608=CARTESIAN_POINT('',(4.,-7.27562663373442E-17,4.5941));
#26609=CARTESIAN_POINT('Ctrl Pts',(20.0288454112575,-0.000266600559035268,
4.5949350414008));
#26610=CARTESIAN_POINT('Ctrl Pts',(20.0141521649359,0.181839152323842,4.59391190659116));
#26611=CARTESIAN_POINT('Ctrl Pts',(19.9994589186142,0.364814066967773,4.50413264800542));
#26612=CARTESIAN_POINT('Ctrl Pts',(19.9847656722925,0.474598868642052,4.35899217880197));
#26613=CARTESIAN_POINT('Ctrl Pts',(19.9688603936049,0.593439717564554,4.20187920587587));
#26614=CARTESIAN_POINT('Ctrl Pts',(19.9529551149173,0.626517665065843,3.97989492921597));
#26615=CARTESIAN_POINT('Ctrl Pts',(19.9370498362297,0.558641803885684,3.79496194153783));
#26616=CARTESIAN_POINT('Ctrl Pts',(19.9211445575421,0.490765942705524,3.61002895385969));
#26617=CARTESIAN_POINT('Ctrl Pts',(19.9052392788545,0.321936272843916,3.46214725516331));
#26618=CARTESIAN_POINT('Ctrl Pts',(19.8893340001669,0.129673778938228,3.41921955761011));
#26619=CARTESIAN_POINT('Ctrl Pts',(19.8734287214793,-0.0625887149674591,
3.37629186005692));
#26620=CARTESIAN_POINT('Ctrl Pts',(19.8575234427916,-0.278284032917226,
3.43831816364691));
#26621=CARTESIAN_POINT('Ctrl Pts',(19.841618164104,-0.418374827314372,3.57681771754473));
#26622=CARTESIAN_POINT('Ctrl Pts',(19.8257128854164,-0.558465621711518,
3.71531727144255));
#26623=CARTESIAN_POINT('Ctrl Pts',(19.8098076067288,-0.622951892556044,
3.9302900756482));
#26624=CARTESIAN_POINT('Ctrl Pts',(19.7939023280412,-0.58222383973146,4.12303018792675));
#26625=CARTESIAN_POINT('Ctrl Pts',(19.7779970493536,-0.541495786906873,
4.3157703002053));
#26626=CARTESIAN_POINT('Ctrl Pts',(19.762091770666,-0.395553410413165,4.48627772055676));
#26627=CARTESIAN_POINT('Ctrl Pts',(19.7461864919784,-0.211407504401025,
4.55626240372308));
#26628=CARTESIAN_POINT('Ctrl Pts',(19.7404061317381,-0.144484459893097,
4.58169651826758));
#26629=CARTESIAN_POINT('Ctrl Pts',(19.7346257714978,-0.0725156072563085,
4.59385388977766));
#26630=CARTESIAN_POINT('Ctrl Pts',(19.7288454112575,-0.000401422265437046,
4.59340756962635));
#26631=CARTESIAN_POINT('Ctrl Pts',(19.6211545887425,0.000364945106097663,
4.59334757974602));
#26632=CARTESIAN_POINT('Ctrl Pts',(19.6310344686986,-0.122924963130536,
4.59265841784648));
#26633=CARTESIAN_POINT('Ctrl Pts',(19.6409143486547,-0.246598186964828,
4.55523353708024));
#26634=CARTESIAN_POINT('Ctrl Pts',(19.6507942286109,-0.346136160298313,
4.48405653351353));
#26635=CARTESIAN_POINT('Ctrl Pts',(19.6666995072985,-0.506378917588675,
4.36947112529969));
#26636=CARTESIAN_POINT('Ctrl Pts',(19.6826047859861,-0.60407113804621,4.16741144784858));
#26637=CARTESIAN_POINT('Ctrl Pts',(19.6985100646737,-0.5943566574826,3.97065479758251));
#26638=CARTESIAN_POINT('Ctrl Pts',(19.7144153433613,-0.584642176918989,
3.77389814731645));
#26639=CARTESIAN_POINT('Ctrl Pts',(19.7303206220489,-0.467520995334232,
3.58244452423543));
#26640=CARTESIAN_POINT('Ctrl Pts',(19.7462259007365,-0.296770260159971,
3.48420125495101));
#26641=CARTESIAN_POINT('Ctrl Pts',(19.7621311794242,-0.12601952498572,3.38595798566659));
#26642=CARTESIAN_POINT('Ctrl Pts',(19.7780364581118,0.098360763778029,3.38092507017875));
#26643=CARTESIAN_POINT('Ctrl Pts',(19.7939417367994,0.27334477570878,3.47141355644931));
#26644=CARTESIAN_POINT('Ctrl Pts',(19.809847015487,0.448328787639532,3.56190204271987));
#26645=CARTESIAN_POINT('Ctrl Pts',(19.8257522941746,0.573916522737285,3.74791193074883));
#26646=CARTESIAN_POINT('Ctrl Pts',(19.8416575728622,0.592443207149574,3.9440350735258));
#26647=CARTESIAN_POINT('Ctrl Pts',(19.8575628515498,0.610969891561863,4.14015821630277));
#26648=CARTESIAN_POINT('Ctrl Pts',(19.8734681302375,0.522435525288687,4.34639461382776));
#26649=CARTESIAN_POINT('Ctrl Pts',(19.8893734089251,0.367491719635661,4.46804975837363));
#26650=CARTESIAN_POINT('Ctrl Pts',(19.8999671355309,0.264291244586565,4.54907828775811));
#26651=CARTESIAN_POINT('Ctrl Pts',(19.9105608621367,0.131629953687138,4.59258455010229));
#26652=CARTESIAN_POINT('Ctrl Pts',(19.9211545887425,-0.000461335262921832,
4.59353843444423));
#26653=CARTESIAN_POINT('Origin',(4.,0.,4.));
#26654=CARTESIAN_POINT('',(20.3288454112575,0.000547175593784699,4.59423670486774));
#26655=CARTESIAN_POINT('',(20.2211545887425,-0.000159442692484791,4.59503650419094));
#26656=CARTESIAN_POINT('',(4.,-7.27562663373442E-17,4.5941));
#26657=CARTESIAN_POINT('Ctrl Pts',(20.3288454112575,0.000547175593784699,
4.59423670486774));
#26658=CARTESIAN_POINT('Ctrl Pts',(20.3254891157492,0.0422991098545892,
4.59465405164581));
#26659=CARTESIAN_POINT('Ctrl Pts',(20.3221328202408,0.0839734681026259,
4.59066114403672));
#26660=CARTESIAN_POINT('Ctrl Pts',(20.3187765247324,0.124636177719752,4.58197547152207));
#26661=CARTESIAN_POINT('Ctrl Pts',(20.3028712460448,0.317334266145104,4.54081460186972));
#26662=CARTESIAN_POINT('Ctrl Pts',(20.2869659673572,0.48731321493246,4.39426577643889));
#26663=CARTESIAN_POINT('Ctrl Pts',(20.2710606886696,0.556778600406793,4.20989870881916));
#26664=CARTESIAN_POINT('Ctrl Pts',(20.255155409982,0.626243985881127,4.02553164119943));
#26665=CARTESIAN_POINT('Ctrl Pts',(20.2392501312944,0.595195808042437,3.80334633139079));
#26666=CARTESIAN_POINT('Ctrl Pts',(20.2233448526068,0.477757630702126,3.64521515909767));
#26667=CARTESIAN_POINT('Ctrl Pts',(20.2074395739191,0.360319453361808,3.48708398680455));
#26668=CARTESIAN_POINT('Ctrl Pts',(20.1915342952315,0.156491276519859,3.39300695202695));
#26669=CARTESIAN_POINT('Ctrl Pts',(20.1756290165439,-0.04006765138094,3.40625706061923));
#26670=CARTESIAN_POINT('Ctrl Pts',(20.1597237378563,-0.236626579281727,
3.4195071692115));
#26671=CARTESIAN_POINT('Ctrl Pts',(20.1438184591687,-0.425916258241364,
3.54008442117362));
#26672=CARTESIAN_POINT('Ctrl Pts',(20.1279131804811,-0.521059912873915,
3.71258420787224));
#26673=CARTESIAN_POINT('Ctrl Pts',(20.1120079017935,-0.616203567506467,
3.88508399457085));
#26674=CARTESIAN_POINT('Ctrl Pts',(20.0961026231058,-0.617201197811932,
4.10950631600596));
#26675=CARTESIAN_POINT('Ctrl Pts',(20.0801973444182,-0.523575121773085,
4.28282745216878));
#26676=CARTESIAN_POINT('Ctrl Pts',(20.0642920657306,-0.429949045734243,
4.45614858833159));
#26677=CARTESIAN_POINT('Ctrl Pts',(20.048386787043,-0.241699263351099,4.57836853922213));
#26678=CARTESIAN_POINT('Ctrl Pts',(20.0324815083554,-0.0452724969876719,
4.59335768007126));
#26679=CARTESIAN_POINT('Ctrl Pts',(20.0312694759895,-0.030304158296608,
4.59449989984645));
#26680=CARTESIAN_POINT('Ctrl Pts',(20.0300574436235,-0.0152883365109376,
4.5950194388496));
#26681=CARTESIAN_POINT('Ctrl Pts',(20.0288454112575,-0.000266600559035268,
4.5949350414008));
#26682=CARTESIAN_POINT('Ctrl Pts',(19.9211545887425,-0.000461335262921832,
4.59353843444423));
#26683=CARTESIAN_POINT('Ctrl Pts',(19.9264661408243,-0.0666901315043342,
4.5940166992278));
#26684=CARTESIAN_POINT('Ctrl Pts',(19.9317776929061,-0.132775635823809,
4.58379778651276));
#26685=CARTESIAN_POINT('Ctrl Pts',(19.9370892449879,-0.194932679790098,
4.56224768701753));
#26686=CARTESIAN_POINT('Ctrl Pts',(19.9529945236755,-0.381060028529917,
4.49771657954882));
#26687=CARTESIAN_POINT('Ctrl Pts',(19.9688998023631,-0.531961480976676,
4.33158047304464));
#26688=CARTESIAN_POINT('Ctrl Pts',(19.9848050810507,-0.578348134104426,
4.14012389605102));
#26689=CARTESIAN_POINT('Ctrl Pts',(20.0007103597384,-0.624734787232175,
3.94866731905739));
#26690=CARTESIAN_POINT('Ctrl Pts',(20.016615638426,-0.566606641040915,3.73189027157431));
#26691=CARTESIAN_POINT('Ctrl Pts',(20.0325209171136,-0.430656211588969,
3.58932409618151));
#26692=CARTESIAN_POINT('Ctrl Pts',(20.0484261958012,-0.294705782137024,
3.44675792078871));
#26693=CARTESIAN_POINT('Ctrl Pts',(20.0643314744888,-0.080933069424392,
3.37840261748619));
#26694=CARTESIAN_POINT('Ctrl Pts',(20.0802367531764,0.112511319004002,3.41565067076361));
#26695=CARTESIAN_POINT('Ctrl Pts',(20.096142031864,0.305955707432406,3.45289872404102));
#26696=CARTESIAN_POINT('Ctrl Pts',(20.1120473105516,0.479071771576571,3.59575013389837));
#26697=CARTESIAN_POINT('Ctrl Pts',(20.1279525892393,0.552362916535151,3.77860107435498));
#26698=CARTESIAN_POINT('Ctrl Pts',(20.1438578679269,0.625654061493722,3.96145201481158));
#26699=CARTESIAN_POINT('Ctrl Pts',(20.1597631466145,0.599120287266732,4.18430248586742));
#26700=CARTESIAN_POINT('Ctrl Pts',(20.1756684253021,0.484961816589866,4.3448525870839));
#26701=CARTESIAN_POINT('Ctrl Pts',(20.1908304797822,0.376137759761604,4.49790047950022));
#26702=CARTESIAN_POINT('Ctrl Pts',(20.2059925342623,0.187686755696174,4.59433432972249));
#26703=CARTESIAN_POINT('Ctrl Pts',(20.2211545887425,-0.000159442692484791,
4.59503650419094));
#26704=CARTESIAN_POINT('Origin',(4.,0.,4.));
#26705=CARTESIAN_POINT('',(20.6288454112575,1.84392275237588E-6,4.59415158619139));
#26706=CARTESIAN_POINT('',(20.5211545887425,0.00014515264107467,4.59408556636595));
#26707=CARTESIAN_POINT('',(4.,-7.27562663373442E-17,4.5941));
#26708=CARTESIAN_POINT('Ctrl Pts',(20.6288454112575,1.84392275237588E-6,
4.59415158619139));
#26709=CARTESIAN_POINT('Ctrl Pts',(20.6209207878748,0.0985777406598016,
4.59414764832452));
#26710=CARTESIAN_POINT('Ctrl Pts',(20.6129961644921,0.197149291092008,4.56908802213256));
#26711=CARTESIAN_POINT('Ctrl Pts',(20.6050715411094,0.283761277174982,4.52200793915563));
#26712=CARTESIAN_POINT('Ctrl Pts',(20.5971189017656,0.370679463050262,4.47476141372331));
#26713=CARTESIAN_POINT('Ctrl Pts',(20.5891662624218,0.445553373684486,4.40533845822152));
#26714=CARTESIAN_POINT('Ctrl Pts',(20.581213623078,0.499196468040806,4.3222224876916));
#26715=CARTESIAN_POINT('Ctrl Pts',(20.5732609837342,0.552839562397126,4.23910651716169));
#26716=CARTESIAN_POINT('Ctrl Pts',(20.5653083443904,0.585251840475543,4.14229753160364));
#26717=CARTESIAN_POINT('Ctrl Pts',(20.5573557050466,0.592531230276538,4.04364021904617));
#26718=CARTESIAN_POINT('Ctrl Pts',(20.5494030657028,0.599810620077534,3.9449829064887));
#26719=CARTESIAN_POINT('Ctrl Pts',(20.541450426359,0.581957121601108,3.84447726693182));
#26720=CARTESIAN_POINT('Ctrl Pts',(20.5334977870152,0.541038843355354,3.75439549632807));
#26721=CARTESIAN_POINT('Ctrl Pts',(20.5255451476714,0.5001205651096,3.66431372572433));
#26722=CARTESIAN_POINT('Ctrl Pts',(20.5175925083276,0.436137507094518,3.58465582407373));
#26723=CARTESIAN_POINT('Ctrl Pts',(20.5096398689838,0.357128912623608,3.5251911792601));
#26724=CARTESIAN_POINT('Ctrl Pts',(20.50168722964,0.278120318152698,3.46572653444646));
#26725=CARTESIAN_POINT('Ctrl Pts',(20.4937345902962,0.184086187225959,3.42645514646979));
#26726=CARTESIAN_POINT('Ctrl Pts',(20.4857819509524,0.0861162623359374,
3.4121221101222));
#26727=CARTESIAN_POINT('Ctrl Pts',(20.4778293116085,-0.0118536625540841,
3.39778907377461));
#26728=CARTESIAN_POINT('Ctrl Pts',(20.4698766722647,-0.113759381407388,
3.4083943890561));
#26729=CARTESIAN_POINT('Ctrl Pts',(20.4619240329209,-0.206384677702653,
3.44274365129583));
#26730=CARTESIAN_POINT('Ctrl Pts',(20.4539713935771,-0.299009973997917,
3.47709291353557));
#26731=CARTESIAN_POINT('Ctrl Pts',(20.4460187542333,-0.382354847735142,
3.53518612273354));
#26732=CARTESIAN_POINT('Ctrl Pts',(20.4380661148895,-0.447563842371028,
3.60976099223211));
#26733=CARTESIAN_POINT('Ctrl Pts',(20.4301134755457,-0.512772837006921,
3.68433586173069));
#26734=CARTESIAN_POINT('Ctrl Pts',(20.4221608362019,-0.559845952541473,
3.77539239152987));
#26735=CARTESIAN_POINT('Ctrl Pts',(20.4142081968581,-0.580888308445953,
3.87190852591559));
#26736=CARTESIAN_POINT('Ctrl Pts',(20.3983029181705,-0.622973020254908,
4.06494079468701));
#26737=CARTESIAN_POINT('Ctrl Pts',(20.3823976394829,-0.5609346935436,4.27981148180459));
#26738=CARTESIAN_POINT('Ctrl Pts',(20.3664923607953,-0.422206916156273,
4.41936036842645));
#26739=CARTESIAN_POINT('Ctrl Pts',(20.353943377616,-0.312753156865475,4.52946196836027));
#26740=CARTESIAN_POINT('Ctrl Pts',(20.3413943944368,-0.155560747392339,
4.59267627084609));
#26741=CARTESIAN_POINT('Ctrl Pts',(20.3288454112575,0.000547175593784699,
4.59423670486774));
#26742=CARTESIAN_POINT('Ctrl Pts',(20.2211545887425,-0.000159442692484791,
4.59503650419094));
#26743=CARTESIAN_POINT('Ctrl Pts',(20.22189781295,-0.00936741923094289,
4.59507092387091));
#26744=CARTESIAN_POINT('Ctrl Pts',(20.2226410371574,-0.0185739425223631,
4.59487531632137));
#26745=CARTESIAN_POINT('Ctrl Pts',(20.2233842613649,-0.0277695625699301,
4.59444507412072));
#26746=CARTESIAN_POINT('Ctrl Pts',(20.2392895400526,-0.224559303926058,
4.58523772856393));
#26747=CARTESIAN_POINT('Ctrl Pts',(20.2551948187402,-0.416355619511548,
4.46857330607325));
#26748=CARTESIAN_POINT('Ctrl Pts',(20.2711000974278,-0.51503297954037,4.29810345018796));
#26749=CARTESIAN_POINT('Ctrl Pts',(20.2870053761154,-0.613710339569191,
4.12763359430267));
#26750=CARTESIAN_POINT('Ctrl Pts',(20.302910654803,-0.619268744041345,3.90335830502277));
#26751=CARTESIAN_POINT('Ctrl Pts',(20.3188159334906,-0.529271009537506,
3.72809546473432));
#26752=CARTESIAN_POINT('Ctrl Pts',(20.3347212121782,-0.439273275033663,
3.55283262444587));
#26753=CARTESIAN_POINT('Ctrl Pts',(20.3506264908658,-0.253719401553817,
3.42658223314887));
#26754=CARTESIAN_POINT('Ctrl Pts',(20.3665317695535,-0.0575887485100287,
3.40762076142476));
#26755=CARTESIAN_POINT('Ctrl Pts',(20.3824370482411,0.138541904533748,3.38865928970065));
#26756=CARTESIAN_POINT('Ctrl Pts',(20.3983423269287,0.345249337141466,3.47698673754941));
#26757=CARTESIAN_POINT('Ctrl Pts',(20.4142476056163,0.467192899405167,3.63141813202173));
#26758=CARTESIAN_POINT('Ctrl Pts',(20.4301528843039,0.589136461668875,3.78584952649406));
#26759=CARTESIAN_POINT('Ctrl Pts',(20.4460581629915,0.626316153588557,4.00638486758996));
#26760=CARTESIAN_POINT('Ctrl Pts',(20.4619634416791,0.562534942182983,4.19337293359078));
#26761=CARTESIAN_POINT('Ctrl Pts',(20.4699160810229,0.530644336480201,4.28686696659118));
#26762=CARTESIAN_POINT('Ctrl Pts',(20.4778687203667,0.473513504946115,4.3719741808178));
#26763=CARTESIAN_POINT('Ctrl Pts',(20.4858213597105,0.400240502138227,4.43864269813793));
#26764=CARTESIAN_POINT('Ctrl Pts',(20.4937739990544,0.326967499330329,4.50531121545807));
#26765=CARTESIAN_POINT('Ctrl Pts',(20.5017266383982,0.237552325248626,4.55354103587171));
#26766=CARTESIAN_POINT('Ctrl Pts',(20.509679277742,0.141619450488441,4.57712494713439));
#26767=CARTESIAN_POINT('Ctrl Pts',(20.5135043814088,0.0954771353210092,
4.58846846487098));
#26768=CARTESIAN_POINT('Ctrl Pts',(20.5173294850756,0.0478269697500401,
4.59411022582368));
#26769=CARTESIAN_POINT('Ctrl Pts',(20.5211545887425,0.00014515264107467,
4.59408556636595));
#26770=CARTESIAN_POINT('Origin',(4.,0.,4.));
#26771=CARTESIAN_POINT('',(20.9288454112575,-6.4040329070536E-6,4.59405282094147));
#26772=CARTESIAN_POINT('',(20.8211545887425,5.65245430726296E-6,4.59414685459231));
#26773=CARTESIAN_POINT('',(4.,-7.27562663373442E-17,4.5941));
#26774=CARTESIAN_POINT('Ctrl Pts',(20.9288454112575,-6.4040329070536E-6,
4.59405282094147));
#26775=CARTESIAN_POINT('Ctrl Pts',(20.9243050993443,0.0564994875152707,
4.59403151438501));
#26776=CARTESIAN_POINT('Ctrl Pts',(20.9197647874311,0.113011285737041,4.58603249222448));
#26777=CARTESIAN_POINT('Ctrl Pts',(20.9152244755179,0.167207550221224,4.57013805289591));
#26778=CARTESIAN_POINT('Ctrl Pts',(20.9072718361741,0.262135685878584,4.5422979516059));
#26779=CARTESIAN_POINT('Ctrl Pts',(20.8993191968303,0.349959832061366,4.49023494241839));
#26780=CARTESIAN_POINT('Ctrl Pts',(20.8913665574865,0.419942299057043,4.42031443844746));
#26781=CARTESIAN_POINT('Ctrl Pts',(20.8834139181427,0.489924766052721,4.35039393447653));
#26782=CARTESIAN_POINT('Ctrl Pts',(20.8754612787989,0.542065553861293,4.26261593572219));
#26783=CARTESIAN_POINT('Ctrl Pts',(20.8675086394551,0.569989725359365,4.16771249585991));
#26784=CARTESIAN_POINT('Ctrl Pts',(20.8595560001113,0.597913896857441,4.07280905599763));
#26785=CARTESIAN_POINT('Ctrl Pts',(20.8516033607674,0.601621452045013,3.97078017502742));
#26786=CARTESIAN_POINT('Ctrl Pts',(20.8436507214236,0.580659121393648,3.87410027737825));
#26787=CARTESIAN_POINT('Ctrl Pts',(20.8356980820798,0.559696790742287,3.77742037972911));
#26788=CARTESIAN_POINT('Ctrl Pts',(20.827745442736,0.514064574252002,3.686089465401));
#26789=CARTESIAN_POINT('Ctrl Pts',(20.8197928033922,0.44934157601673,3.61127397478397));
#26790=CARTESIAN_POINT('Ctrl Pts',(20.8118401640484,0.384618577781443,3.53645848416692));
#26791=CARTESIAN_POINT('Ctrl Pts',(20.8038875247046,0.300804797801161,3.47815841726095));
#26792=CARTESIAN_POINT('Ctrl Pts',(20.7959348853608,0.208147717693743,3.44350176598286));
#26793=CARTESIAN_POINT('Ctrl Pts',(20.787982246017,0.115490637586335,3.40884511470477));
#26794=CARTESIAN_POINT('Ctrl Pts',(20.7800296066732,0.0139902573517945,
3.39783187905454));
#26795=CARTESIAN_POINT('Ctrl Pts',(20.7720769673294,-0.0839438183138644,
3.41180854931868));
#26796=CARTESIAN_POINT('Ctrl Pts',(20.7641243279856,-0.181877893979523,
3.42578521958283));
#26797=CARTESIAN_POINT('Ctrl Pts',(20.7561716886418,-0.2762456650763,3.46475179576135));
#26798=CARTESIAN_POINT('Ctrl Pts',(20.748219049298,-0.355509010203556,3.52394413563581));
#26799=CARTESIAN_POINT('Ctrl Pts',(20.7402664099542,-0.434772355330821,
3.58313647551028));
#26800=CARTESIAN_POINT('Ctrl Pts',(20.7323137706103,-0.498931274488562,
3.66255457908069));
#26801=CARTESIAN_POINT('Ctrl Pts',(20.7243611312665,-0.54014217617541,3.75248840252759));
#26802=CARTESIAN_POINT('Ctrl Pts',(20.7164084919227,-0.581353077862249,
3.84242222597448));
#26803=CARTESIAN_POINT('Ctrl Pts',(20.7084558525789,-0.599615962078206,
3.94287176929784));
#26804=CARTESIAN_POINT('Ctrl Pts',(20.7005032132351,-0.592696601504336,
4.0415558946729));
#26805=CARTESIAN_POINT('Ctrl Pts',(20.6925505738913,-0.585777240930466,
4.14024002004797));
#26806=CARTESIAN_POINT('Ctrl Pts',(20.6845979345475,-0.553675635566762,
4.23715872747472));
#26807=CARTESIAN_POINT('Ctrl Pts',(20.6766452952037,-0.50031917594212,4.32046203197985));
#26808=CARTESIAN_POINT('Ctrl Pts',(20.6686926558599,-0.446962716317479,
4.40376533648498));
#26809=CARTESIAN_POINT('Ctrl Pts',(20.6607400165161,-0.3723514024319,4.47345323806848));
#26810=CARTESIAN_POINT('Ctrl Pts',(20.6527873771723,-0.285602702553558,
4.52100610813718));
#26811=CARTESIAN_POINT('Ctrl Pts',(20.6448347378285,-0.198854002675205,
4.56855897820588));
#26812=CARTESIAN_POINT('Ctrl Pts',(20.6368820984847,-0.099967916804087,
4.59397681675976));
#26813=CARTESIAN_POINT('Ctrl Pts',(20.6289294591409,-0.00104364331035449,
4.59415068835528));
#26814=CARTESIAN_POINT('Ctrl Pts',(20.6289014431798,-0.000695147863829354,
4.59415130087895));
#26815=CARTESIAN_POINT('Ctrl Pts',(20.6288734272186,-0.000346651943377611,
4.59415160011295));
#26816=CARTESIAN_POINT('Ctrl Pts',(20.6288454112575,1.84392275237588E-6,
4.59415158619139));
#26817=CARTESIAN_POINT('Ctrl Pts',(20.5211545887425,0.00014515264107467,
4.59408556636595));
#26818=CARTESIAN_POINT('Ctrl Pts',(20.5252821244194,-0.0513066296901884,
4.59405895720698));
#26819=CARTESIAN_POINT('Ctrl Pts',(20.5294096600964,-0.102795266482965,
4.58743447362686));
#26820=CARTESIAN_POINT('Ctrl Pts',(20.5335371957734,-0.152465997634008,
4.57425651377355));
#26821=CARTESIAN_POINT('Ctrl Pts',(20.5414898351172,-0.248167995557571,
4.5488661670383));
#26822=CARTESIAN_POINT('Ctrl Pts',(20.549442474461,-0.33712141596603,4.49914747145609));
#26823=CARTESIAN_POINT('Ctrl Pts',(20.5573951138048,-0.408848640915227,
4.43107686705031));
#26824=CARTESIAN_POINT('Ctrl Pts',(20.5653477531486,-0.480575865864423,
4.36300626264453));
#26825=CARTESIAN_POINT('Ctrl Pts',(20.5733003924924,-0.535076895354358,
4.27658374941519));
#26826=CARTESIAN_POINT('Ctrl Pts',(20.5812530318362,-0.565476628275392,
4.18243021985824));
#26827=CARTESIAN_POINT('Ctrl Pts',(20.58920567118,-0.595876361196427,4.08827669030129));
#26828=CARTESIAN_POINT('Ctrl Pts',(20.5971583105238,-0.602174797548561,
3.98639214441672));
#26829=CARTESIAN_POINT('Ctrl Pts',(20.6051109498677,-0.58371402745925,3.88920441471463));
#26830=CARTESIAN_POINT('Ctrl Pts',(20.6130635892115,-0.565253257369939,
3.79201668501254));
#26831=CARTESIAN_POINT('Ctrl Pts',(20.6210162285553,-0.522033280839182,
3.69952577149293));
#26832=CARTESIAN_POINT('Ctrl Pts',(20.6289688678991,-0.459278917219465,
3.62305528060961));
#26833=CARTESIAN_POINT('Ctrl Pts',(20.6369215072429,-0.396524553599749,
3.54658478972629));
#26834=CARTESIAN_POINT('Ctrl Pts',(20.6448741465867,-0.314235802891072,
3.48613472147926));
#26835=CARTESIAN_POINT('Ctrl Pts',(20.6528267859305,-0.222505051509483,
3.44908779917463));
#26836=CARTESIAN_POINT('Ctrl Pts',(20.6607794252743,-0.130774300127894,
3.41204087687));
#26837=CARTESIAN_POINT('Ctrl Pts',(20.6687320646181,-0.029601548073392,
3.39839710050778));
#26838=CARTESIAN_POINT('Ctrl Pts',(20.6766847039619,0.0686601223983595,
3.40982890848785));
#26839=CARTESIAN_POINT('Ctrl Pts',(20.6846373433057,0.1669217928701,3.42126071646792));
#26840=CARTESIAN_POINT('Ctrl Pts',(20.6925899826495,0.262272381759091,3.45776810879028));
#26841=CARTESIAN_POINT('Ctrl Pts',(20.7005426219933,0.343045155251024,3.51488528173127));
#26842=CARTESIAN_POINT('Ctrl Pts',(20.7084952613371,0.423817928742975,3.57200245467228));
#26843=CARTESIAN_POINT('Ctrl Pts',(20.7164479006809,0.490012886837861,3.64972940823193));
#26844=CARTESIAN_POINT('Ctrl Pts',(20.7244005400247,0.533541468465666,3.73856417004634));
#26845=CARTESIAN_POINT('Ctrl Pts',(20.7323531793686,0.577070050093471,3.82739893186076));
#26846=CARTESIAN_POINT('Ctrl Pts',(20.7403058187123,0.597932255254196,3.92734150192994));
#26847=CARTESIAN_POINT('Ctrl Pts',(20.7482584580562,0.593574919799613,4.02617190099588));
#26848=CARTESIAN_POINT('Ctrl Pts',(20.7562110974,0.589217584345031,4.1250023000618));
#26849=CARTESIAN_POINT('Ctrl Pts',(20.7641637367438,0.559640708275147,4.22272052812447));
#26850=CARTESIAN_POINT('Ctrl Pts',(20.7721163760876,0.508461778515953,4.30737953925928));
#26851=CARTESIAN_POINT('Ctrl Pts',(20.7800690154314,0.457282848756759,4.39203855039408));
#26852=CARTESIAN_POINT('Ctrl Pts',(20.7880216547752,0.384501865308254,4.46363834460102));
#26853=CARTESIAN_POINT('Ctrl Pts',(20.795974294119,0.299016600344635,4.51342469267633));
#26854=CARTESIAN_POINT('Ctrl Pts',(20.8039269334628,0.213531335381016,4.56321104075164));
#26855=CARTESIAN_POINT('Ctrl Pts',(20.8118795728066,0.115341788902283,4.59118394269532));
#26856=CARTESIAN_POINT('Ctrl Pts',(20.8198322121504,0.0164533379892873,
4.59392342516246));
#26857=CARTESIAN_POINT('Ctrl Pts',(20.8202730043478,0.0109722321971217,
4.59407526688998));
#26858=CARTESIAN_POINT('Ctrl Pts',(20.8207137965451,0.00548897925183007,
4.59414958726715));
#26859=CARTESIAN_POINT('Ctrl Pts',(20.8211545887425,5.65245430726296E-6,
4.59414685459231));
#26860=CARTESIAN_POINT('Origin',(4.,0.,4.));
#26861=CARTESIAN_POINT('',(21.2288454112575,1.28243205298473E-5,4.59412621697841));
#26862=CARTESIAN_POINT('',(21.1211545887425,-1.09306879613159E-5,4.5940621922514));
#26863=CARTESIAN_POINT('',(4.,-7.27562663373442E-17,4.5941));
#26864=CARTESIAN_POINT('Ctrl Pts',(21.2288454112575,1.28243205298473E-5,
4.59412621697841));
#26865=CARTESIAN_POINT('Ctrl Pts',(21.2276894108138,0.0143945780386088,
4.59413985249388));
#26866=CARTESIAN_POINT('Ctrl Pts',(21.2265334103701,0.028775363636007,4.59362827285675));
#26867=CARTESIAN_POINT('Ctrl Pts',(21.2253774099263,0.043117441953227,4.59258471957415));
#26868=CARTESIAN_POINT('Ctrl Pts',(21.2174247705826,0.141782954511012,4.58540565408365));
#26869=CARTESIAN_POINT('Ctrl Pts',(21.2094721312387,0.238616577754522,4.55305001116024));
#26870=CARTESIAN_POINT('Ctrl Pts',(21.2015194918949,0.321779082392626,4.49947370882601));
#26871=CARTESIAN_POINT('Ctrl Pts',(21.1935668525511,0.404941587030731,4.44589740649178));
#26872=CARTESIAN_POINT('Ctrl Pts',(21.1856142132073,0.474432973063433,4.37110044474674));
#26873=CARTESIAN_POINT('Ctrl Pts',(21.1776615738635,0.521756972098598,4.28422777087894));
#26874=CARTESIAN_POINT('Ctrl Pts',(21.1697089345197,0.569080971133768,4.19735509701114));
#26875=CARTESIAN_POINT('Ctrl Pts',(21.1617562951759,0.594237583171398,4.09840671102057));
#26876=CARTESIAN_POINT('Ctrl Pts',(21.1538036558321,0.594151069756079,3.9994804007435));
#26877=CARTESIAN_POINT('Ctrl Pts',(21.1458510164883,0.59406455634076,3.90055409046644));
#26878=CARTESIAN_POINT('Ctrl Pts',(21.1378983771445,0.568734917472505,3.80164985590287));
#26879=CARTESIAN_POINT('Ctrl Pts',(21.1299457378007,0.521259046500119,3.71486008677882));
#26880=CARTESIAN_POINT('Ctrl Pts',(21.1219930984569,0.473783175527722,3.62807031765475));
#26881=CARTESIAN_POINT('Ctrl Pts',(21.114040459113,0.40416107245118,3.5533950139702));
#26882=CARTESIAN_POINT('Ctrl Pts',(21.1060878197692,0.320904987578411,3.49996424865404));
#26883=CARTESIAN_POINT('Ctrl Pts',(21.0981351804254,0.237648902705652,3.44653348333788));
#26884=CARTESIAN_POINT('Ctrl Pts',(21.0901825410817,0.140758836036697,3.41434725639011));
#26885=CARTESIAN_POINT('Ctrl Pts',(21.0822299017378,0.042080917889342,3.40734077242984));
#26886=CARTESIAN_POINT('Ctrl Pts',(21.074277262394,-0.056597000258024,3.40033428846957));
#26887=CARTESIAN_POINT('Ctrl Pts',(21.0663246230502,-0.157062769883762,
3.41850754749682));
#26888=CARTESIAN_POINT('Ctrl Pts',(21.0583719837064,-0.247033082431791,
3.45963862106718));
#26889=CARTESIAN_POINT('Ctrl Pts',(21.0504193443626,-0.337003394979799,
3.50076969463752));
#26890=CARTESIAN_POINT('Ctrl Pts',(21.0424667050188,-0.416478250450111,
3.56485858275095));
#26891=CARTESIAN_POINT('Ctrl Pts',(21.034514065675,-0.475740765152555,3.644069545988));
#26892=CARTESIAN_POINT('Ctrl Pts',(21.0265614263312,-0.535003279855012,
3.72328050922507));
#26893=CARTESIAN_POINT('Ctrl Pts',(21.0186087869874,-0.574053453789596,
3.81761354758578));
#26894=CARTESIAN_POINT('Ctrl Pts',(21.0106561476436,-0.588116871685884,
3.91553516229212));
#26895=CARTESIAN_POINT('Ctrl Pts',(21.0027035082998,-0.60218028958217,4.01345677699845));
#26896=CARTESIAN_POINT('Ctrl Pts',(20.994750868956,-0.591256951440166,4.11496696805043));
#26897=CARTESIAN_POINT('Ctrl Pts',(20.9867982296121,-0.556682383467722,
4.20765473214191));
#26898=CARTESIAN_POINT('Ctrl Pts',(20.9788455902683,-0.522107815495282,
4.30034249623339));
#26899=CARTESIAN_POINT('Ctrl Pts',(20.9708929509246,-0.463882017692404,
4.38420783336438));
#26900=CARTESIAN_POINT('Ctrl Pts',(20.9629403115808,-0.389123888092725,
4.4489970636758));
#26901=CARTESIAN_POINT('Ctrl Pts',(20.9549876722369,-0.314365758493028,
4.51378629398723));
#26902=CARTESIAN_POINT('Ctrl Pts',(20.9470350328931,-0.223075297096518,
4.5594994174791));
#26903=CARTESIAN_POINT('Ctrl Pts',(20.9390823935493,-0.12641400383229,4.58054738252877));
#26904=CARTESIAN_POINT('Ctrl Pts',(20.9356700661187,-0.0849384674446181,
4.58957866703598));
#26905=CARTESIAN_POINT('Ctrl Pts',(20.9322577386881,-0.0424741039190781,
4.59406883414683));
#26906=CARTESIAN_POINT('Ctrl Pts',(20.9288454112575,-6.4040329070536E-6,
4.59405282094147));
#26907=CARTESIAN_POINT('Ctrl Pts',(20.8211545887425,5.65245430726296E-6,
4.59414685459231));
#26908=CARTESIAN_POINT('Ctrl Pts',(20.8286664358889,-0.0934395423672534,
4.59410028517524));
#26909=CARTESIAN_POINT('Ctrl Pts',(20.8361782830354,-0.18690618531264,4.57167601133058));
#26910=CARTESIAN_POINT('Ctrl Pts',(20.8436901301818,-0.270133012248912,
4.529191754035));
#26911=CARTESIAN_POINT('Ctrl Pts',(20.8516427695256,-0.358243556226857,
4.4842145374498));
#26912=CARTESIAN_POINT('Ctrl Pts',(20.8595954088694,-0.434877288835492,
4.41675404128879));
#26913=CARTESIAN_POINT('Ctrl Pts',(20.8675480482133,-0.490664589397756,
4.33505825661903));
#26914=CARTESIAN_POINT('Ctrl Pts',(20.8755006875571,-0.546451889960021,
4.25336247194927));
#26915=CARTESIAN_POINT('Ctrl Pts',(20.8834533269009,-0.581392758475918,
4.15743139877076));
#26916=CARTESIAN_POINT('Ctrl Pts',(20.8914059662447,-0.591215252505097,
4.05899390323763));
#26917=CARTESIAN_POINT('Ctrl Pts',(20.8993586055885,-0.601037746534278,
3.96055640770449));
#26918=CARTESIAN_POINT('Ctrl Pts',(20.9073112449323,-0.585741866076735,
3.85961248981672));
#26919=CARTESIAN_POINT('Ctrl Pts',(20.9152638842761,-0.547197711916726,
3.76850392583047));
#26920=CARTESIAN_POINT('Ctrl Pts',(20.9232165236199,-0.508653557756717,
3.67739536184422));
#26921=CARTESIAN_POINT('Ctrl Pts',(20.9311691629637,-0.446861129894262,
3.59612215175949));
#26922=CARTESIAN_POINT('Ctrl Pts',(20.9391218023075,-0.369375409551539,
3.53462104847409));
#26923=CARTESIAN_POINT('Ctrl Pts',(20.9470744416513,-0.291889689208826,
3.4731199451887));
#26924=CARTESIAN_POINT('Ctrl Pts',(20.9550270809951,-0.198710676385865,
3.43139094870266));
#26925=CARTESIAN_POINT('Ctrl Pts',(20.9629797203389,-0.101230766359376,
3.41453599926792));
#26926=CARTESIAN_POINT('Ctrl Pts',(20.9709323596827,-0.00375085633288601,
3.39768104983318));
#26927=CARTESIAN_POINT('Ctrl Pts',(20.9788849990265,0.0980299508971346,
3.40570014744973));
#26928=CARTESIAN_POINT('Ctrl Pts',(20.9868376383704,0.191667561123074,3.43761284710704));
#26929=CARTESIAN_POINT('Ctrl Pts',(20.9947902777142,0.285305171349014,3.46952554676435));
#26930=CARTESIAN_POINT('Ctrl Pts',(21.002742917058,0.37079958457088,3.52533184846243));
#26931=CARTESIAN_POINT('Ctrl Pts',(21.0106955564018,0.437697946637459,3.59820867233944));
#26932=CARTESIAN_POINT('Ctrl Pts',(21.0186481957456,0.504596308704037,3.67108549621644));
#26933=CARTESIAN_POINT('Ctrl Pts',(21.0266008350894,0.552898619615334,3.76103284227238));
#26934=CARTESIAN_POINT('Ctrl Pts',(21.0345534744332,0.576699262792956,3.8570534220826));
#26935=CARTESIAN_POINT('Ctrl Pts',(21.042506113777,0.600499905970578,3.95307400189282));
#26936=CARTESIAN_POINT('Ctrl Pts',(21.0504587531208,0.599798881414527,4.05516781545734));
#26937=CARTESIAN_POINT('Ctrl Pts',(21.0584113924646,0.574681899562831,4.15085250374278));
#26938=CARTESIAN_POINT('Ctrl Pts',(21.0663640318084,0.549564917711138,4.24653719202821));
#26939=CARTESIAN_POINT('Ctrl Pts',(21.0743166711522,0.500031978563804,4.33581275503458));
#26940=CARTESIAN_POINT('Ctrl Pts',(21.082269310496,0.432139158218639,4.40776403918836));
#26941=CARTESIAN_POINT('Ctrl Pts',(21.0902219498398,0.364246337873458,4.47971532334216));
#26942=CARTESIAN_POINT('Ctrl Pts',(21.0981745891836,0.277993636330433,4.53434232864337));
#26943=CARTESIAN_POINT('Ctrl Pts',(21.1061272285274,0.183926621270441,4.56496615973523));
#26944=CARTESIAN_POINT('Ctrl Pts',(21.1111363485991,0.124676735433976,4.5842551580617));
#26945=CARTESIAN_POINT('Ctrl Pts',(21.1161454686708,0.0623266393968894,
4.59402126159141));
#26946=CARTESIAN_POINT('Ctrl Pts',(21.1211545887425,-1.09306879613159E-5,
4.5940621922514));
#26947=CARTESIAN_POINT('Origin',(4.,0.,4.));
#26948=CARTESIAN_POINT('',(21.5288454112575,-1.51073027558624E-5,4.59408477831653));
#26949=CARTESIAN_POINT('',(21.4211545887425,1.51733402061755E-5,4.59410821609125));
#26950=CARTESIAN_POINT('',(4.,-7.27562663373442E-17,4.5941));
#26951=CARTESIAN_POINT('Ctrl Pts',(21.5288454112575,-1.51073027558624E-5,
4.59408477831653));
#26952=CARTESIAN_POINT('Ctrl Pts',(21.5231210829395,0.0712153309254728,
4.59401644885886));
#26953=CARTESIAN_POINT('Ctrl Pts',(21.5173967546214,0.142469702059594,4.58119587380047));
#26954=CARTESIAN_POINT('Ctrl Pts',(21.5116724263034,0.209120766622247,4.55613331912479));
#26955=CARTESIAN_POINT('Ctrl Pts',(21.5037197869596,0.301717111362981,4.52131465616629));
#26956=CARTESIAN_POINT('Ctrl Pts',(21.4957671476158,0.385428743083265,4.46286809139133));
#26957=CARTESIAN_POINT('Ctrl Pts',(21.4878145082719,0.450020774675764,4.38793951336988));
#26958=CARTESIAN_POINT('Ctrl Pts',(21.4798618689281,0.514612806268249,4.31301093534845));
#26959=CARTESIAN_POINT('Ctrl Pts',(21.4719092295843,0.560085237732952,4.22160034408054));
#26960=CARTESIAN_POINT('Ctrl Pts',(21.4639565902405,0.58087844500124,4.1248839293359));
#26961=CARTESIAN_POINT('Ctrl Pts',(21.4560039508967,0.601671652269532,4.02816751459124));
#26962=CARTESIAN_POINT('Ctrl Pts',(21.4480513115529,0.597785635341394,3.92614527636987));
#26963=CARTESIAN_POINT('Ctrl Pts',(21.4400986722091,0.569695512712777,3.83129082280931));
#26964=CARTESIAN_POINT('Ctrl Pts',(21.4321460328653,0.541605390084162,3.73643636924876));
#26965=CARTESIAN_POINT('Ctrl Pts',(21.4241933935215,0.489311161755075,3.64874970034904));
#26966=CARTESIAN_POINT('Ctrl Pts',(21.4162407541777,0.419206509371839,3.57895170565158));
#26967=CARTESIAN_POINT('Ctrl Pts',(21.4082881148339,0.349101856988603,3.50915371095413));
#26968=CARTESIAN_POINT('Ctrl Pts',(21.4003354754901,0.261186780551223,3.45724439045894));
#26969=CARTESIAN_POINT('Ctrl Pts',(21.3923828361463,0.16621009553345,3.42957036558731));
#26970=CARTESIAN_POINT('Ctrl Pts',(21.3844301968025,0.0712334105156764,
3.40189634071567));
#26971=CARTESIAN_POINT('Ctrl Pts',(21.3764775574587,-0.0308048830825163,
3.3984576114676));
#26972=CARTESIAN_POINT('Ctrl Pts',(21.3685249181149,-0.127429214135013,
3.41967460932821));
#26973=CARTESIAN_POINT('Ctrl Pts',(21.360572278771,-0.22405354518751,3.44089160718882));
#26974=CARTESIAN_POINT('Ctrl Pts',(21.3526196394272,-0.315263913694308,
3.4867643321581));
#26975=CARTESIAN_POINT('Ctrl Pts',(21.3446670000834,-0.389908609845283,
3.5516842188346));
#26976=CARTESIAN_POINT('Ctrl Pts',(21.3367143607396,-0.464553305996249,
3.6166041055111));
#26977=CARTESIAN_POINT('Ctrl Pts',(21.3287617213958,-0.522632329791381,
3.70057115389483));
#26978=CARTESIAN_POINT('Ctrl Pts',(21.320809082052,-0.557044729551177,3.79331924871262));
#26979=CARTESIAN_POINT('Ctrl Pts',(21.3128564427082,-0.591457129310977,
3.88606734353042));
#26980=CARTESIAN_POINT('Ctrl Pts',(21.3049038033644,-0.602202905035458,
3.9875964847823));
#26981=CARTESIAN_POINT('Ctrl Pts',(21.2969511640206,-0.587968239287942,
4.08549335215105));
#26982=CARTESIAN_POINT('Ctrl Pts',(21.2889985246768,-0.573733573540424,
4.18339021951981));
#26983=CARTESIAN_POINT('Ctrl Pts',(21.281045885333,-0.534518466320906,4.27765481300544));
#26984=CARTESIAN_POINT('Ctrl Pts',(21.2730932459892,-0.47511749858569,4.35676200219639));
#26985=CARTESIAN_POINT('Ctrl Pts',(21.2651406066454,-0.415716530850488,
4.43586919138732));
#26986=CARTESIAN_POINT('Ctrl Pts',(21.2571879673016,-0.336129702599601,
4.49981897628356));
#26987=CARTESIAN_POINT('Ctrl Pts',(21.2492353279577,-0.246087587538132,
4.54079262470289));
#26988=CARTESIAN_POINT('Ctrl Pts',(21.2424386890577,-0.169134048541188,
4.57581031891556));
#26989=CARTESIAN_POINT('Ctrl Pts',(21.2356420501576,-0.0845438791841879,
4.59404604774026));
#26990=CARTESIAN_POINT('Ctrl Pts',(21.2288454112575,1.28243205298473E-5,
4.59412621697841));
#26991=CARTESIAN_POINT('Ctrl Pts',(21.1211545887425,-1.09306879613159E-5,
4.5940621922514));
#26992=CARTESIAN_POINT('Ctrl Pts',(21.1240981080146,-0.0366424819978743,
4.5940862444172));
#26993=CARTESIAN_POINT('Ctrl Pts',(21.1270416272867,-0.0732697079540161,
4.59075208378119));
#26994=CARTESIAN_POINT('Ctrl Pts',(21.1299851465589,-0.109260984540888,
4.58401866488291));
#26995=CARTESIAN_POINT('Ctrl Pts',(21.1379377859027,-0.20650024671525,4.56582668205621));
#26996=CARTESIAN_POINT('Ctrl Pts',(21.1458904252465,-0.299097442487026,
4.52282205952027));
#26997=CARTESIAN_POINT('Ctrl Pts',(21.1538430645903,-0.375731303474415,
4.46026269810429));
#26998=CARTESIAN_POINT('Ctrl Pts',(21.1617957039341,-0.452365164461805,
4.3977033366883));
#26999=CARTESIAN_POINT('Ctrl Pts',(21.1697483432779,-0.513035690664809,
4.31558923639226));
#27000=CARTESIAN_POINT('Ctrl Pts',(21.1777009826217,-0.550325083965727,
4.22395996434209));
#27001=CARTESIAN_POINT('Ctrl Pts',(21.1856536219655,-0.587614477266646,
4.13233069229192));
#27002=CARTESIAN_POINT('Ctrl Pts',(21.1936062613093,-0.601522737665479,
4.03118624848761));
#27003=CARTESIAN_POINT('Ctrl Pts',(21.2015589006531,-0.590349390887683,
3.93289291874755));
#27004=CARTESIAN_POINT('Ctrl Pts',(21.2095115399969,-0.579176044109886,
3.83459958900749));
#27005=CARTESIAN_POINT('Ctrl Pts',(21.2174641793407,-0.542921090155459,
3.73915737333167));
#27006=CARTESIAN_POINT('Ctrl Pts',(21.2254168186845,-0.486017190935348,
3.65823538248142));
#27007=CARTESIAN_POINT('Ctrl Pts',(21.2333694580283,-0.429113291715238,
3.57731339163117));
#27008=CARTESIAN_POINT('Ctrl Pts',(21.2413220973721,-0.351560447229444,
3.51091162560648));
#27009=CARTESIAN_POINT('Ctrl Pts',(21.249274736716,-0.262840548960938,3.46714860467879));
#27010=CARTESIAN_POINT('Ctrl Pts',(21.2572273760598,-0.174120650692433,
3.4233855837511));
#27011=CARTESIAN_POINT('Ctrl Pts',(21.2651800154036,-0.0742336986412151,
3.40226130792041));
#27012=CARTESIAN_POINT('Ctrl Pts',(21.2731326547474,0.0246077668693877,
3.40635850761334));
#27013=CARTESIAN_POINT('Ctrl Pts',(21.2810852940912,0.123449232380002,3.41045570730627));
#27014=CARTESIAN_POINT('Ctrl Pts',(21.289037933435,0.221245211350001,3.43977438252282));
#27015=CARTESIAN_POINT('Ctrl Pts',(21.2969905727788,0.306038813396919,3.49072992590572));
#27016=CARTESIAN_POINT('Ctrl Pts',(21.3049432121226,0.390832415443818,3.54168546928862));
#27017=CARTESIAN_POINT('Ctrl Pts',(21.3128958514664,0.462623640567642,3.61427788083785));
#27018=CARTESIAN_POINT('Ctrl Pts',(21.3208484908102,0.512635033719562,3.69963174955258));
#27019=CARTESIAN_POINT('Ctrl Pts',(21.328801130154,0.562646426871494,3.78498561826733));
#27020=CARTESIAN_POINT('Ctrl Pts',(21.3367537694978,0.590877988051513,3.88310094414759));
#27021=CARTESIAN_POINT('Ctrl Pts',(21.3447064088416,0.59387802439953,3.98198179230066));
#27022=CARTESIAN_POINT('Ctrl Pts',(21.3526590481854,0.596878060747546,4.08086264045372));
#27023=CARTESIAN_POINT('Ctrl Pts',(21.3606116875293,0.574646572263566,4.1805090108796));
#27024=CARTESIAN_POINT('Ctrl Pts',(21.3685643268731,0.529901661201384,4.26873777763737));
#27025=CARTESIAN_POINT('Ctrl Pts',(21.3765169662169,0.485156750139203,4.35696654439514));
#27026=CARTESIAN_POINT('Ctrl Pts',(21.3844696055607,0.417898416498819,4.4337777074848));
#27027=CARTESIAN_POINT('Ctrl Pts',(21.3924222449045,0.336349907607971,4.48978005607163));
#27028=CARTESIAN_POINT('Ctrl Pts',(21.4003748842483,0.254801398717122,4.54578240465847));
#27029=CARTESIAN_POINT('Ctrl Pts',(21.4083275235921,0.158962714575808,4.58097593874246));
#27030=CARTESIAN_POINT('Ctrl Pts',(21.4162801629359,0.0605514396169286,
4.59105776945554));
#27031=CARTESIAN_POINT('Ctrl Pts',(21.4179049715381,0.0404449719157324,
4.59311759444699));
#27032=CARTESIAN_POINT('Ctrl Pts',(21.4195297801403,0.0202311170044278,
4.59412918598148));
#27033=CARTESIAN_POINT('Ctrl Pts',(21.4211545887425,1.51733402061755E-5,
4.59410821609125));
#27034=CARTESIAN_POINT('Origin',(4.,0.,4.));
#27035=CARTESIAN_POINT('',(21.8288454112575,1.47252919898561E-5,4.59408074293421));
#27036=CARTESIAN_POINT('',(21.7211545887425,-1.54601956517634E-5,4.59410286710644));
#27037=CARTESIAN_POINT('',(4.,-7.27562663373442E-17,4.5941));
#27038=CARTESIAN_POINT('Ctrl Pts',(21.8288454112575,1.47252919898561E-5,
4.59408074293421));
#27039=CARTESIAN_POINT('Ctrl Pts',(21.826505394409,0.0291331941223908,4.59410767674242));
#27040=CARTESIAN_POINT('Ctrl Pts',(21.8241653775604,0.0582478076928112,
4.59200528777341));
#27041=CARTESIAN_POINT('Ctrl Pts',(21.8218253607118,0.0870422430987805,
4.58774093918134));
#27042=CARTESIAN_POINT('Ctrl Pts',(21.813872721368,0.184901264939656,4.57324838268129));
#27043=CARTESIAN_POINT('Ctrl Pts',(21.8059200820242,0.279062206656402,4.53378504179028));
#27044=CARTESIAN_POINT('Ctrl Pts',(21.7979674426804,0.358012610677869,4.47417584741217));
#27045=CARTESIAN_POINT('Ctrl Pts',(21.7900148033366,0.436963014699336,4.41456665303406));
#27046=CARTESIAN_POINT('Ctrl Pts',(21.7820621639928,0.500702881025523,4.33481160516884));
#27047=CARTESIAN_POINT('Ctrl Pts',(21.774109524649,0.541439142878506,4.24466184465998));
#27048=CARTESIAN_POINT('Ctrl Pts',(21.7661568853052,0.58217540473149,4.15451208415111));
#27049=CARTESIAN_POINT('Ctrl Pts',(21.7582042459614,0.599908062111268,4.0539676109986));
#27050=CARTESIAN_POINT('Ctrl Pts',(21.7502516066176,0.59246905613922,3.95532135643358));
#27051=CARTESIAN_POINT('Ctrl Pts',(21.7422989672738,0.585030050167171,3.85667510186855));
#27052=CARTESIAN_POINT('Ctrl Pts',(21.73434632793,0.552419380843296,3.759927065891));
#27053=CARTESIAN_POINT('Ctrl Pts',(21.7263936885861,0.498624146640836,3.67690601358098));
#27054=CARTESIAN_POINT('Ctrl Pts',(21.7184410492423,0.444828912438376,3.59388496127097));
#27055=CARTESIAN_POINT('Ctrl Pts',(21.7104884098985,0.369849113357332,3.52459089262848));
#27056=CARTESIAN_POINT('Ctrl Pts',(21.7025357705547,0.28285205103972,3.47749595131133));
#27057=CARTESIAN_POINT('Ctrl Pts',(21.6945831312109,0.195854988722108,3.43040100999418));
#27058=CARTESIAN_POINT('Ctrl Pts',(21.6866304918671,0.0968406631679286,
3.40550519600236));
#27059=CARTESIAN_POINT('Ctrl Pts',(21.6786778525233,-0.00208507577578169,
3.40585236167057));
#27060=CARTESIAN_POINT('Ctrl Pts',(21.6707252131795,-0.101010814719503,
3.40619952733877));
#27061=CARTESIAN_POINT('Ctrl Pts',(21.6627725738357,-0.199847967052756,
3.431789672667));
#27062=CARTESIAN_POINT('Ctrl Pts',(21.6548199344919,-0.28651234476781,3.47949405385809));
#27063=CARTESIAN_POINT('Ctrl Pts',(21.6468672951481,-0.373176722482865,
3.52719843504918));
#27064=CARTESIAN_POINT('Ctrl Pts',(21.6389146558043,-0.44766832557972,3.59701705210314));
#27065=CARTESIAN_POINT('Ctrl Pts',(21.6309620164605,-0.500879541024521,
3.68041362817464));
#27066=CARTESIAN_POINT('Ctrl Pts',(21.6230093771167,-0.55409075646931,3.76381020424612));
#27067=CARTESIAN_POINT('Ctrl Pts',(21.6150567377728,-0.586021584262053,
3.86078473933514));
#27068=CARTESIAN_POINT('Ctrl Pts',(21.607104098429,-0.592768045815946,3.95948077576042));
#27069=CARTESIAN_POINT('Ctrl Pts',(21.5991514590852,-0.599514507369841,
4.05817681218572));
#27070=CARTESIAN_POINT('Ctrl Pts',(21.5911988197414,-0.581076602684875,
4.15859434994728));
#27071=CARTESIAN_POINT('Ctrl Pts',(21.5832461803976,-0.539708616728004,
4.24845597739434));
#27072=CARTESIAN_POINT('Ctrl Pts',(21.5752935410538,-0.498340630771147,
4.33831760484137));
#27073=CARTESIAN_POINT('Ctrl Pts',(21.56734090171,-0.434042563542403,4.41762332197391));
#27074=CARTESIAN_POINT('Ctrl Pts',(21.5593882623662,-0.354675729482573,
4.47667692475034));
#27075=CARTESIAN_POINT('Ctrl Pts',(21.5514356230224,-0.275308895422716,
4.53573052752678));
#27076=CARTESIAN_POINT('Ctrl Pts',(21.5434829836786,-0.180873294531764,
4.57453201594709));
#27077=CARTESIAN_POINT('Ctrl Pts',(21.5355303443348,-0.0829149652056982,
4.58833737958621));
#27078=CARTESIAN_POINT('Ctrl Pts',(21.533302033309,-0.055467269432644,4.59220561033096));
#27079=CARTESIAN_POINT('Ctrl Pts',(21.5310737222833,-0.0277430016607059,
4.5941113769453));
#27080=CARTESIAN_POINT('Ctrl Pts',(21.5288454112575,-1.51073027558624E-5,
4.59408477831653));
#27081=CARTESIAN_POINT('Ctrl Pts',(21.4211545887425,1.51733402061755E-5,
4.59410821609125));
#27082=CARTESIAN_POINT('Ctrl Pts',(21.4274824194841,-0.0787159889745399,
4.59402654867773));
#27083=CARTESIAN_POINT('Ctrl Pts',(21.4338102502257,-0.15747883181342,4.57828382012605));
#27084=CARTESIAN_POINT('Ctrl Pts',(21.4401380809673,-0.230053504748576,
4.54780575811717));
#27085=CARTESIAN_POINT('Ctrl Pts',(21.4480907203111,-0.321263308378747,
4.50950178872359));
#27086=CARTESIAN_POINT('Ctrl Pts',(21.4560433596549,-0.402699049862651,
4.44792372259427));
#27087=CARTESIAN_POINT('Ctrl Pts',(21.4639959989987,-0.464404100671371,
4.37060031698995));
#27088=CARTESIAN_POINT('Ctrl Pts',(21.4719486383425,-0.526109151480106,
4.2932769113856));
#27089=CARTESIAN_POINT('Ctrl Pts',(21.4799012776864,-0.568083511613643,
4.20020816630624));
#27090=CARTESIAN_POINT('Ctrl Pts',(21.4878539170302,-0.585195243866348,
4.10277300340868));
#27091=CARTESIAN_POINT('Ctrl Pts',(21.495806556374,-0.602306976119048,4.00533784051114));
#27092=CARTESIAN_POINT('Ctrl Pts',(21.5037591957178,-0.594556080490919,
3.90353625979537));
#27093=CARTESIAN_POINT('Ctrl Pts',(21.5117118350616,-0.562890209537588,
3.80981489101362));
#27094=CARTESIAN_POINT('Ctrl Pts',(21.5196644744054,-0.53122433858425,3.71609352223184));
#27095=CARTESIAN_POINT('Ctrl Pts',(21.5276171137492,-0.47564349230572,3.63045236538409));
#27096=CARTESIAN_POINT('Ctrl Pts',(21.535569753093,-0.402943186155437,3.56336221830407));
#27097=CARTESIAN_POINT('Ctrl Pts',(21.5435223924368,-0.330242880005154,
3.49627207122406));
#27098=CARTESIAN_POINT('Ctrl Pts',(21.5514750317806,-0.24042311398314,3.44773293391182));
#27099=CARTESIAN_POINT('Ctrl Pts',(21.5594276711244,-0.144465577806233,
3.42367937699355));
#27100=CARTESIAN_POINT('Ctrl Pts',(21.5673803104682,-0.0485080416293372,
3.39962582007528));
#27101=CARTESIAN_POINT('Ctrl Pts',(21.575332949812,0.0535872647024426,3.40005784355098));
#27102=CARTESIAN_POINT('Ctrl Pts',(21.5832855891558,0.149337799479898,3.42492262666669));
#27103=CARTESIAN_POINT('Ctrl Pts',(21.5912382284996,0.245088334257342,3.44978740978241));
#27104=CARTESIAN_POINT('Ctrl Pts',(21.5991908678434,0.33449409748049,3.49908495253815));
#27105=CARTESIAN_POINT('Ctrl Pts',(21.6071435071872,0.406624016913212,3.56678795891296));
#27106=CARTESIAN_POINT('Ctrl Pts',(21.6150961465311,0.478753936345942,3.63449096528778));
#27107=CARTESIAN_POINT('Ctrl Pts',(21.6230487858749,0.533608011988269,3.72059943528167));
#27108=CARTESIAN_POINT('Ctrl Pts',(21.6310014252187,0.564479585995414,3.81458543566408));
#27109=CARTESIAN_POINT('Ctrl Pts',(21.6389540645625,0.595351160002559,3.90857143604649));
#27110=CARTESIAN_POINT('Ctrl Pts',(21.6469067039063,0.602240232374519,4.0104349668174));
#27111=CARTESIAN_POINT('Ctrl Pts',(21.6548593432501,0.584304520186539,4.10772182398666));
#27112=CARTESIAN_POINT('Ctrl Pts',(21.6628119825939,0.566368807998562,4.2050086811559));
#27113=CARTESIAN_POINT('Ctrl Pts',(21.6707646219377,0.523608311250652,4.29771886472347));
#27114=CARTESIAN_POINT('Ctrl Pts',(21.6787172612815,0.461251083056512,4.37451729206089));
#27115=CARTESIAN_POINT('Ctrl Pts',(21.6866699006253,0.398893854862358,4.45131571939834));
#27116=CARTESIAN_POINT('Ctrl Pts',(21.6946225399691,0.316939895221968,4.51220239050563));
#27117=CARTESIAN_POINT('Ctrl Pts',(21.7025751793129,0.225409191891896,4.54973308058009));
#27118=CARTESIAN_POINT('Ctrl Pts',(21.7087683157894,0.15412944274098,4.5789601931952));
#27119=CARTESIAN_POINT('Ctrl Pts',(21.7149614522659,0.0770418275534371,
4.59402294959611));
#27120=CARTESIAN_POINT('Ctrl Pts',(21.7211545887425,-1.54601956517634E-5,
4.59410286710644));
#27121=CARTESIAN_POINT('Origin',(4.,0.,4.));
#27122=CARTESIAN_POINT('',(22.1288454112575,-1.19684274697274E-5,4.59413016891312));
#27123=CARTESIAN_POINT('',(22.0211545887425,1.20066176157995E-5,4.59406577061205));
#27124=CARTESIAN_POINT('',(4.,-7.27562663373442E-17,4.5941));
#27125=CARTESIAN_POINT('Ctrl Pts',(22.1288454112575,-1.19684274697274E-5,
4.59413016891312));
#27126=CARTESIAN_POINT('Ctrl Pts',(22.1219370665346,0.0859328098890183,
4.59405244111828));
#27127=CARTESIAN_POINT('Ctrl Pts',(22.1150287218117,0.171910584533005,4.57519344187135));
#27128=CARTESIAN_POINT('Ctrl Pts',(22.1081203770888,0.24987714748571,4.53905210772026));
#27129=CARTESIAN_POINT('Ctrl Pts',(22.100167737745,0.339629466009183,4.49744749656716));
#27130=CARTESIAN_POINT('Ctrl Pts',(22.0922150984012,0.418765494330909,4.4329406966096));
#27131=CARTESIAN_POINT('Ctrl Pts',(22.0842624590574,0.477609775176754,4.35341854270704));
#27132=CARTESIAN_POINT('Ctrl Pts',(22.0763098197136,0.536454056022584,4.2738963888045));
#27133=CARTESIAN_POINT('Ctrl Pts',(22.0683571803698,0.575006589392542,4.17935888095698));
#27134=CARTESIAN_POINT('Ctrl Pts',(22.060404541026,0.588553803007579,4.081364517074));
#27135=CARTESIAN_POINT('Ctrl Pts',(22.0524519016822,0.60210101662262,3.983370153191));
#27136=CARTESIAN_POINT('Ctrl Pts',(22.0444992623384,0.590642910482727,3.88191893327255));
#27137=CARTESIAN_POINT('Ctrl Pts',(22.0365466229946,0.55558039411957,3.78941465069146));
#27138=CARTESIAN_POINT('Ctrl Pts',(22.0285939836508,0.520517877756421,3.69691036811039));
#27139=CARTESIAN_POINT('Ctrl Pts',(22.020641344307,0.461850951170019,3.61335302286667));
#27140=CARTESIAN_POINT('Ctrl Pts',(22.0126887049632,0.386752445163155,3.5489586384446));
#27141=CARTESIAN_POINT('Ctrl Pts',(22.0047360656194,0.311653939156274,3.48456425402251));
#27142=CARTESIAN_POINT('Ctrl Pts',(21.9967834262756,0.220123853728924,3.43933283042207));
#27143=CARTESIAN_POINT('Ctrl Pts',(21.9888307869318,0.123352988439278,3.41879452521803));
#27144=CARTESIAN_POINT('Ctrl Pts',(21.980878147588,0.0265821231496428,3.398256220014));
#27145=CARTESIAN_POINT('Ctrl Pts',(21.9729255082441,-0.075429522002288,
3.40241103320635));
#27146=CARTESIAN_POINT('Ctrl Pts',(21.9649728689003,-0.170209634025949,
3.43075098229493));
#27147=CARTESIAN_POINT('Ctrl Pts',(21.9570202295565,-0.26498974604961,3.4590909313835));
#27148=CARTESIAN_POINT('Ctrl Pts',(21.9490675902127,-0.352538324945002,
3.5116160163683));
#27149=CARTESIAN_POINT('Ctrl Pts',(21.9411149508689,-0.422151364554475,
3.58190433023263));
#27150=CARTESIAN_POINT('Ctrl Pts',(21.9331623115251,-0.491764404163956,
3.65219264409696));
#27151=CARTESIAN_POINT('Ctrl Pts',(21.9252096721813,-0.543441904487514,
3.74024418684083));
#27152=CARTESIAN_POINT('Ctrl Pts',(21.9172570328375,-0.570865587277161,
3.83529345812586));
#27153=CARTESIAN_POINT('Ctrl Pts',(21.9093043934937,-0.598289270066803,
3.93034272941087));
#27154=CARTESIAN_POINT('Ctrl Pts',(21.9013517541499,-0.601459135322544,
4.03238972923704));
#27155=CARTESIAN_POINT('Ctrl Pts',(21.8933991148061,-0.579987623844179,
4.12895782202339));
#27156=CARTESIAN_POINT('Ctrl Pts',(21.8854464754623,-0.558516112365809,
4.22552591480976));
#27157=CARTESIAN_POINT('Ctrl Pts',(21.8774938361185,-0.512403224153321,
4.31661510055631));
#27158=CARTESIAN_POINT('Ctrl Pts',(21.8695411967747,-0.447286887835617,
4.39108848569571));
#27159=CARTESIAN_POINT('Ctrl Pts',(21.8615885574308,-0.38217055151792,4.46556187083511));
#27160=CARTESIAN_POINT('Ctrl Pts',(21.853635918087,-0.298050767095013,4.52341945536736));
#27161=CARTESIAN_POINT('Ctrl Pts',(21.8456832787432,-0.205212323901057,
4.55758736157894));
#27162=CARTESIAN_POINT('Ctrl Pts',(21.840070656248,-0.139691040693493,4.58170156451555));
#27163=CARTESIAN_POINT('Ctrl Pts',(21.8344580337528,-0.0698270680627233,
4.59401614113532));
#27164=CARTESIAN_POINT('Ctrl Pts',(21.8288454112575,1.47252919898561E-5,
4.59408074293421));
#27165=CARTESIAN_POINT('Ctrl Pts',(21.7211545887425,-1.54601956517634E-5,
4.59410286710644));
#27166=CARTESIAN_POINT('Ctrl Pts',(21.7229140916097,-0.0219078436841643,
4.59412557209431));
#27167=CARTESIAN_POINT('Ctrl Pts',(21.724673594477,-0.0437977792686499,
4.59293892497318));
#27168=CARTESIAN_POINT('Ctrl Pts',(21.7264330973443,-0.0655513867134097,
4.59052415646896));
#27169=CARTESIAN_POINT('Ctrl Pts',(21.7343857366881,-0.163873814968881,
4.57960983324176));
#27170=CARTESIAN_POINT('Ctrl Pts',(21.742338376032,-0.259411224460086,4.54360647774573));
#27171=CARTESIAN_POINT('Ctrl Pts',(21.7502910153758,-0.340482865683332,
4.48691599054611));
#27172=CARTESIAN_POINT('Ctrl Pts',(21.7582436547196,-0.421554506906578,
4.4302255033465));
#27173=CARTESIAN_POINT('Ctrl Pts',(21.7661962940634,-0.488160379861865,
4.3528478844433));
#27174=CARTESIAN_POINT('Ctrl Pts',(21.7741489334072,-0.532157009426634,
4.26424360160945));
#27175=CARTESIAN_POINT('Ctrl Pts',(21.782101572751,-0.576153638991403,4.1756393187756));
#27176=CARTESIAN_POINT('Ctrl Pts',(21.7900542120948,-0.597541025165654,
4.0758083720111));
#27177=CARTESIAN_POINT('Ctrl Pts',(21.7980068514386,-0.593704268699233,
3.9769564542281));
#27178=CARTESIAN_POINT('Ctrl Pts',(21.8059594907824,-0.589867512232813,
3.87810453644509));
#27179=CARTESIAN_POINT('Ctrl Pts',(21.8139121301262,-0.560806613125721,
3.78023164764359));
#27180=CARTESIAN_POINT('Ctrl Pts',(21.82186476947,-0.510074662095298,3.69530408148155));
#27181=CARTESIAN_POINT('Ctrl Pts',(21.8298174088138,-0.459342711064876,
3.61037651531951));
#27182=CARTESIAN_POINT('Ctrl Pts',(21.8377700481576,-0.386939708111122,
3.53839427179695));
#27183=CARTESIAN_POINT('Ctrl Pts',(21.8457226875014,-0.301717906454235,
3.48815816056295));
#27184=CARTESIAN_POINT('Ctrl Pts',(21.8536753268452,-0.216496104797349,
3.43792204932895));
#27185=CARTESIAN_POINT('Ctrl Pts',(21.8616279661891,-0.118455504437329,
3.40943207038352));
#27186=CARTESIAN_POINT('Ctrl Pts',(21.8695806055329,-0.0195829040543552,
3.40617151167847));
#27187=CARTESIAN_POINT('Ctrl Pts',(21.8775332448767,0.0792896963286298,
3.40291095297342));
#27188=CARTESIAN_POINT('Ctrl Pts',(21.8854858842205,0.178994296734569,3.42487981450875));
#27189=CARTESIAN_POINT('Ctrl Pts',(21.8934385235643,0.267340651814441,3.46939210375187));
#27190=CARTESIAN_POINT('Ctrl Pts',(21.9013911629081,0.355687006894294,3.51390439299499));
#27191=CARTESIAN_POINT('Ctrl Pts',(21.9093438022519,0.432675116648084,3.58096010994589));
#27192=CARTESIAN_POINT('Ctrl Pts',(21.9172964415957,0.488892136101412,3.66236077992681));
#27193=CARTESIAN_POINT('Ctrl Pts',(21.9252490809395,0.545109155554752,3.74376144990775));
#27194=CARTESIAN_POINT('Ctrl Pts',(21.9332017202833,0.580555084707621,3.8395070729187));
#27195=CARTESIAN_POINT('Ctrl Pts',(21.9411543596271,0.590896175957217,3.93789144251738));
#27196=CARTESIAN_POINT('Ctrl Pts',(21.9491069989709,0.601237267206812,4.03627581211605));
#27197=CARTESIAN_POINT('Ctrl Pts',(21.9570596383147,0.58647352055314,4.13729892830245));
#27198=CARTESIAN_POINT('Ctrl Pts',(21.9650122776585,0.548410005102802,4.22860933921557));
#27199=CARTESIAN_POINT('Ctrl Pts',(21.9729649170023,0.510346489652465,4.31991975012869));
#27200=CARTESIAN_POINT('Ctrl Pts',(21.9809175563462,0.448983205405461,4.40151745576853));
#27201=CARTESIAN_POINT('Ctrl Pts',(21.98887019569,0.371822649612145,4.46342602528218));
#27202=CARTESIAN_POINT('Ctrl Pts',(21.9968228350338,0.29466209381883,4.52533459479583));
#27203=CARTESIAN_POINT('Ctrl Pts',(22.0047754743776,0.201704266479203,4.5675540281833));
#27204=CARTESIAN_POINT('Ctrl Pts',(22.0127281137214,0.104314528045707,4.58492242469582));
#27205=CARTESIAN_POINT('Ctrl Pts',(22.0155369387284,0.069917050565085,4.59105683924014));
#27206=CARTESIAN_POINT('Ctrl Pts',(22.0183457637354,0.0349667096964542,
4.59409118517947));
#27207=CARTESIAN_POINT('Ctrl Pts',(22.0211545887425,1.20066176157995E-5,
4.59406577061205));
#27208=CARTESIAN_POINT('Origin',(4.,0.,4.));
#27209=CARTESIAN_POINT('',(22.4288454112575,5.18920962550018E-6,4.59405135764298));
#27210=CARTESIAN_POINT('',(22.3211545887424,-7.30827440488969E-6,4.59414400810326));
#27211=CARTESIAN_POINT('',(4.,-7.27562663373442E-17,4.5941));
#27212=CARTESIAN_POINT('Ctrl Pts',(22.4288454112575,5.18920962550018E-6,
4.59405135764298));
#27213=CARTESIAN_POINT('Ctrl Pts',(22.4253213780041,0.0438634191921666,
4.5940647188338));
#27214=CARTESIAN_POINT('Ctrl Pts',(22.4217973447507,0.0877187745911938,
4.589273164082));
#27215=CARTESIAN_POINT('Ctrl Pts',(22.4182733114973,0.130485535360993,4.57964583089408));
#27216=CARTESIAN_POINT('Ctrl Pts',(22.4103206721535,0.226996720088313,4.55791995512033));
#27217=CARTESIAN_POINT('Ctrl Pts',(22.4023680328097,0.317964089339764,4.51156722320365));
#27218=CARTESIAN_POINT('Ctrl Pts',(22.3944153934659,0.392265646131591,4.44625488916104));
#27219=CARTESIAN_POINT('Ctrl Pts',(22.3864627541221,0.4665672029234,4.38094255511845));
#27220=CARTESIAN_POINT('Ctrl Pts',(22.3785101147783,0.524202947255594,4.29667061894994));
#27221=CARTESIAN_POINT('Ctrl Pts',(22.3705574754345,0.558126122886914,4.20374247196213));
#27222=CARTESIAN_POINT('Ctrl Pts',(22.3626048360906,0.592049298518242,4.11081432497429));
#27223=CARTESIAN_POINT('Ctrl Pts',(22.3546521967468,0.602259905448686,4.00922996716717));
#27224=CARTESIAN_POINT('Ctrl Pts',(22.346699557403,0.587509558716917,3.91140947017845));
#27225=CARTESIAN_POINT('Ctrl Pts',(22.3387469180592,0.572759211985149,3.81358897318973));
#27226=CARTESIAN_POINT('Ctrl Pts',(22.3307942787154,0.533047911591167,3.71953233701942));
#27227=CARTESIAN_POINT('Ctrl Pts',(22.3228416393716,0.473230904440663,3.6407392662825));
#27228=CARTESIAN_POINT('Ctrl Pts',(22.3148890000278,0.413413897290173,3.5619461955456));
#27229=CARTESIAN_POINT('Ctrl Pts',(22.306936360684,0.333491183383171,3.49841669024209));
#27230=CARTESIAN_POINT('Ctrl Pts',(22.2989837213402,0.243234403245124,3.45791809774646));
#27231=CARTESIAN_POINT('Ctrl Pts',(22.2910310819964,0.152977623107077,3.41741950525082));
#27232=CARTESIAN_POINT('Ctrl Pts',(22.2830784426526,0.0523867767379842,
3.39995182556307));
#27233=CARTESIAN_POINT('Ctrl Pts',(22.2751258033088,-0.0462395349927855,
3.40765072037886));
#27234=CARTESIAN_POINT('Ctrl Pts',(22.267173163965,-0.144865846723578,3.41534961519466));
#27235=CARTESIAN_POINT('Ctrl Pts',(22.2592205246212,-0.241527623816046,
3.448215084514));
#27236=CARTESIAN_POINT('Ctrl Pts',(22.2512678852774,-0.324406647450603,
3.50222887712101));
#27237=CARTESIAN_POINT('Ctrl Pts',(22.2433152459336,-0.40728567108515,3.55624266972802));
#27238=CARTESIAN_POINT('Ctrl Pts',(22.2353626065897,-0.476381941261788,
3.63140478562268));
#27239=CARTESIAN_POINT('Ctrl Pts',(22.2274099672459,-0.523247497912515,
3.71852563243507));
#27240=CARTESIAN_POINT('Ctrl Pts',(22.2194573279021,-0.570113054563243,
3.80564647924745));
#27241=CARTESIAN_POINT('Ctrl Pts',(22.2115046885583,-0.59474789768806,3.90472605697756));
#27242=CARTESIAN_POINT('Ctrl Pts',(22.2035520492145,-0.594140082177443,
4.00365053781872));
#27243=CARTESIAN_POINT('Ctrl Pts',(22.1955994098707,-0.593532266666827,
4.10257501865988));
#27244=CARTESIAN_POINT('Ctrl Pts',(22.1876467705269,-0.567681792520777,
4.2013444026121));
#27245=CARTESIAN_POINT('Ctrl Pts',(22.1796941311831,-0.519749232289404,
4.2878827872712));
#27246=CARTESIAN_POINT('Ctrl Pts',(22.1717414918393,-0.471816672058032,
4.37442117193029));
#27247=CARTESIAN_POINT('Ctrl Pts',(22.1637888524955,-0.401802025741336,
4.44872855729627));
#27248=CARTESIAN_POINT('Ctrl Pts',(22.1558362131517,-0.318265537426909,
4.50171985346399));
#27249=CARTESIAN_POINT('Ctrl Pts',(22.1478835738079,-0.234729049112483,
4.55471114963171));
#27250=CARTESIAN_POINT('Ctrl Pts',(22.1399309344641,-0.137670718800326,
4.58638635660118));
#27251=CARTESIAN_POINT('Ctrl Pts',(22.1319782951203,-0.0389572492816432,
4.5928727489116));
#27252=CARTESIAN_POINT('Ctrl Pts',(22.1309340004994,-0.0259947671705595,
4.5937245044491));
#27253=CARTESIAN_POINT('Ctrl Pts',(22.1298897058784,-0.0130037447923657,
4.5941419185755));
#27254=CARTESIAN_POINT('Ctrl Pts',(22.1288454112575,-1.19684274697274E-5,
4.59413016891312));
#27255=CARTESIAN_POINT('Ctrl Pts',(22.0211545887425,1.20066176157995E-5,
4.59406577061205));
#27256=CARTESIAN_POINT('Ctrl Pts',(22.0262984030792,-0.064000704172389,
4.59401922879619));
#27257=CARTESIAN_POINT('Ctrl Pts',(22.031442217416,-0.128028044405449,4.5837112392356));
#27258=CARTESIAN_POINT('Ctrl Pts',(22.0365860317528,-0.188701337098646,
4.56338935830438));
#27259=CARTESIAN_POINT('Ctrl Pts',(22.0445386710966,-0.282505814282095,
4.53197053576284));
#27260=CARTESIAN_POINT('Ctrl Pts',(22.0524913104404,-0.368293119121642,
4.4766155310422));
#27261=CARTESIAN_POINT('Ctrl Pts',(22.0604439497842,-0.435574585201076,
4.40409224738955));
#27262=CARTESIAN_POINT('Ctrl Pts',(22.068396589128,-0.502856051280518,4.33156896373689));
#27263=CARTESIAN_POINT('Ctrl Pts',(22.0763492284718,-0.551631678599843,
4.24187740115222));
#27264=CARTESIAN_POINT('Ctrl Pts',(22.0843018678156,-0.575937982408454,
4.14598357473613));
#27265=CARTESIAN_POINT('Ctrl Pts',(22.0922545071594,-0.600244286217068,
4.05008974832002));
#27266=CARTESIAN_POINT('Ctrl Pts',(22.1002071465032,-0.600081266514962,
3.94799365807249));
#27267=CARTESIAN_POINT('Ctrl Pts',(22.1081597858471,-0.575468854681199,
3.85217794154701));
#27268=CARTESIAN_POINT('Ctrl Pts',(22.1161124251909,-0.550856442847438,
3.75636222502155));
#27269=CARTESIAN_POINT('Ctrl Pts',(22.1240650645347,-0.501794638882025,
3.66682688221814));
#27270=CARTESIAN_POINT('Ctrl Pts',(22.1320177038785,-0.434281916527717,
3.5945188282416));
#27271=CARTESIAN_POINT('Ctrl Pts',(22.1399703432223,-0.366769194173409,
3.52221077426505));
#27272=CARTESIAN_POINT('Ctrl Pts',(22.1479229825661,-0.280805553430205,
3.46713000911538));
#27273=CARTESIAN_POINT('Ctrl Pts',(22.1558756219099,-0.186901220180937,
3.43601090651668));
#27274=CARTESIAN_POINT('Ctrl Pts',(22.1638282612537,-0.0929968869316588,
3.40489180391798));
#27275=CARTESIAN_POINT('Ctrl Pts',(22.1717809005975,0.00884813882368474,
3.39773436387026));
#27276=CARTESIAN_POINT('Ctrl Pts',(22.1797335399413,0.106181915586414,3.41541368090248));
#27277=CARTESIAN_POINT('Ctrl Pts',(22.1876861792851,0.203515692349121,3.4330929979347));
#27278=CARTESIAN_POINT('Ctrl Pts',(22.1956388186289,0.296338220119215,3.47560907204686));
#27279=CARTESIAN_POINT('Ctrl Pts',(22.2035914579727,0.373300680656879,3.53776373412001));
#27280=CARTESIAN_POINT('Ctrl Pts',(22.2115440973165,0.450263141194552,3.59991839619317));
#27281=CARTESIAN_POINT('Ctrl Pts',(22.2194967366603,0.511365534499791,3.68171164622733));
#27282=CARTESIAN_POINT('Ctrl Pts',(22.2274493760041,0.549137260797828,3.7731431454068));
#27283=CARTESIAN_POINT('Ctrl Pts',(22.2354020153479,0.586908987095865,3.86457464458628));
#27284=CARTESIAN_POINT('Ctrl Pts',(22.2433546546918,0.6013500463867,3.96564439291107));
#27285=CARTESIAN_POINT('Ctrl Pts',(22.2513072940356,0.590694822479903,4.06399523710107));
#27286=CARTESIAN_POINT('Ctrl Pts',(22.2592599333794,0.580039598573106,4.16234608129106));
#27287=CARTESIAN_POINT('Ctrl Pts',(22.2672125727232,0.544288091468676,4.25797802134625));
#27288=CARTESIAN_POINT('Ctrl Pts',(22.275165212067,0.487811409852587,4.33919875012361));
#27289=CARTESIAN_POINT('Ctrl Pts',(22.2831178514108,0.431334728236497,4.42041947890096));
#27290=CARTESIAN_POINT('Ctrl Pts',(22.2910704907546,0.354132872108749,4.48722899640046));
#27291=CARTESIAN_POINT('Ctrl Pts',(22.2990231300984,0.265644819817582,4.53145892916239));
#27292=CARTESIAN_POINT('Ctrl Pts',(22.3064002829798,0.183560135512932,4.57248819778762));
#27293=CARTESIAN_POINT('Ctrl Pts',(22.3137774358611,0.0917635873240076,
4.59408754951618));
#27294=CARTESIAN_POINT('Ctrl Pts',(22.3211545887424,-7.30827440488969E-6,
4.59414400810326));
#27295=CARTESIAN_POINT('Origin',(4.,0.,4.));
#27296=CARTESIAN_POINT('',(22.7288454112575,-7.11440487624268E-7,4.59414971000239));
#27297=CARTESIAN_POINT('',(22.6211545887425,-1.51245797256638E-7,4.59404869726453));
#27298=CARTESIAN_POINT('',(4.,-7.27562663373442E-17,4.5941));
#27299=CARTESIAN_POINT('Ctrl Pts',(22.7288454112575,-7.11440487624268E-7,
4.59414971000239));
#27300=CARTESIAN_POINT('Ctrl Pts',(22.7287056894736,0.0017373052546791,
4.59414999869406));
#27301=CARTESIAN_POINT('Ctrl Pts',(22.7285659676897,0.0034753215591825,
4.59414251282321));
#27302=CARTESIAN_POINT('Ctrl Pts',(22.7284262459057,0.00521327185949689,
4.59412723628209));
#27303=CARTESIAN_POINT('Ctrl Pts',(22.7204736065619,0.104133365400505,4.59325773105135));
#27304=CARTESIAN_POINT('Ctrl Pts',(22.7125209672181,0.202839630323109,4.56714939948764));
#27305=CARTESIAN_POINT('Ctrl Pts',(22.7045683278743,0.289252680684759,4.51898953373575));
#27306=CARTESIAN_POINT('Ctrl Pts',(22.6966156885305,0.375665731046408,4.47082966798385));
#27307=CARTESIAN_POINT('Ctrl Pts',(22.6886630491867,0.449785566847107,4.40061826804377));
#27308=CARTESIAN_POINT('Ctrl Pts',(22.6807104098429,0.502555912967013,4.31694216252228));
#27309=CARTESIAN_POINT('Ctrl Pts',(22.6727577704991,0.555326259086918,4.23326605700079));
#27310=CARTESIAN_POINT('Ctrl Pts',(22.6648051311553,0.586747115526033,4.13612524589788));
#27311=CARTESIAN_POINT('Ctrl Pts',(22.6568524918115,0.592973744123511,4.03739517928057));
#27312=CARTESIAN_POINT('Ctrl Pts',(22.6488998524677,0.59920037272099,3.93866511266326));
#27313=CARTESIAN_POINT('Ctrl Pts',(22.6409472131239,0.580232773476834,3.83834579053153));
#27314=CARTESIAN_POINT('Ctrl Pts',(22.6329945737801,0.538391640361539,3.74870332422701));
#27315=CARTESIAN_POINT('Ctrl Pts',(22.6250419344363,0.496550507246239,3.65906085792248));
#27316=CARTESIAN_POINT('Ctrl Pts',(22.6170892950925,0.431835840259791,3.58009524744515));
#27317=CARTESIAN_POINT('Ctrl Pts',(22.6091366557487,0.35215901686313,3.52146073929621));
#27318=CARTESIAN_POINT('Ctrl Pts',(22.6011840164048,0.272482193466486,3.46282623114728));
#27319=CARTESIAN_POINT('Ctrl Pts',(22.593231377061,0.17784321365963,3.42452282532672));
#27320=CARTESIAN_POINT('Ctrl Pts',(22.5852787377172,0.0798134434713266,
3.41123383340666));
#27321=CARTESIAN_POINT('Ctrl Pts',(22.5773260983734,-0.0182163267169884,
3.3979448414866));
#27322=CARTESIAN_POINT('Ctrl Pts',(22.5693734590296,-0.119636887286728,
3.40967026346704));
#27323=CARTESIAN_POINT('Ctrl Pts',(22.5614208196858,-0.212048437952692,
3.44497640167274));
#27324=CARTESIAN_POINT('Ctrl Pts',(22.553468180342,-0.304459988618666,3.48028253987845));
#27325=CARTESIAN_POINT('Ctrl Pts',(22.5455155409982,-0.387862529380837,
3.53916939430943));
#27326=CARTESIAN_POINT('Ctrl Pts',(22.5375629016544,-0.452058834188948,
3.61443730067171));
#27327=CARTESIAN_POINT('Ctrl Pts',(22.5296102623106,-0.516255138997059,
3.689705207034));
#27328=CARTESIAN_POINT('Ctrl Pts',(22.5216576229668,-0.561245207851117,
3.7813541653276));
#27329=CARTESIAN_POINT('Ctrl Pts',(22.513704983623,-0.581528460676763,3.87817881267738));
#27330=CARTESIAN_POINT('Ctrl Pts',(22.5057523442792,-0.601811713502406,
3.97500346002715));
#27331=CARTESIAN_POINT('Ctrl Pts',(22.4977997049354,-0.597388150299644,
4.07700379643311));
#27332=CARTESIAN_POINT('Ctrl Pts',(22.4898470655916,-0.568798575589296,
4.17170890717095));
#27333=CARTESIAN_POINT('Ctrl Pts',(22.4818944262477,-0.540209000878948,
4.26641401790879));
#27334=CARTESIAN_POINT('Ctrl Pts',(22.4739417869039,-0.487453414661012,
4.35382390297851));
#27335=CARTESIAN_POINT('Ctrl Pts',(22.4659891475601,-0.416981925106977,
4.42325150516024));
#27336=CARTESIAN_POINT('Ctrl Pts',(22.4580365082163,-0.346510435552941,
4.49267910734197));
#27337=CARTESIAN_POINT('Ctrl Pts',(22.4500838688725,-0.258323042662803,
4.54412442663572));
#27338=CARTESIAN_POINT('Ctrl Pts',(22.4421312295287,-0.163201846116148,
4.57129757646718));
#27339=CARTESIAN_POINT('Ctrl Pts',(22.4377026234383,-0.11023146834083,4.58642955613285));
#27340=CARTESIAN_POINT('Ctrl Pts',(22.4332740173479,-0.0551108697057404,
4.59403456681078));
#27341=CARTESIAN_POINT('Ctrl Pts',(22.4288454112575,5.18920962550018E-6,
4.59405135764298));
#27342=CARTESIAN_POINT('Ctrl Pts',(22.3211545887424,-7.30827440488969E-6,
4.59414400810326));
#27343=CARTESIAN_POINT('Ctrl Pts',(22.3217300752049,-0.00716629073194701,
4.59414841239758));
#27344=CARTESIAN_POINT('Ctrl Pts',(22.3223055616673,-0.0143251170819474,
4.59402171850555));
#27345=CARTESIAN_POINT('Ctrl Pts',(22.3228810481298,-0.0214791647150919,
4.59376292335171));
#27346=CARTESIAN_POINT('Ctrl Pts',(22.3308336874736,-0.120340848501978,
4.59018663675477));
#27347=CARTESIAN_POINT('Ctrl Pts',(22.3387863268174,-0.218289967621164,
4.56138371553656));
#27348=CARTESIAN_POINT('Ctrl Pts',(22.3467389661612,-0.303350908332583,
4.51087570903952));
#27349=CARTESIAN_POINT('Ctrl Pts',(22.3546916055051,-0.388411849044011,
4.46036770254246));
#27350=CARTESIAN_POINT('Ctrl Pts',(22.3626442448489,-0.460584611347669,
4.38815461076656));
#27351=CARTESIAN_POINT('Ctrl Pts',(22.3705968841927,-0.511045091866278,
4.3030654678256));
#27352=CARTESIAN_POINT('Ctrl Pts',(22.3785495235365,-0.561505572384874,
4.21797632488466));
#27353=CARTESIAN_POINT('Ctrl Pts',(22.3865021628803,-0.590253771118432,
4.12001113077866));
#27354=CARTESIAN_POINT('Ctrl Pts',(22.3944548022241,-0.593774829630164,
4.02114746451658));
#27355=CARTESIAN_POINT('Ctrl Pts',(22.4024074415679,-0.597295888141896,
3.92228379825449));
#27356=CARTESIAN_POINT('Ctrl Pts',(22.4103600809117,-0.575589806431797,
3.82252165983632));
#27357=CARTESIAN_POINT('Ctrl Pts',(22.4183127202555,-0.531310447862662,
3.73405832985033));
#27358=CARTESIAN_POINT('Ctrl Pts',(22.4262653595993,-0.487031089293526,
3.64559499986435));
#27359=CARTESIAN_POINT('Ctrl Pts',(22.4342179989431,-0.420178453865353,
3.56843047831055));
#27360=CARTESIAN_POINT('Ctrl Pts',(22.4421706382869,-0.338926188203527,
3.51199917808983));
#27361=CARTESIAN_POINT('Ctrl Pts',(22.4501232776307,-0.257673922541701,
3.45556787786912));
#27362=CARTESIAN_POINT('Ctrl Pts',(22.4580759169745,-0.162022026646223,
3.41986979898149));
#27363=CARTESIAN_POINT('Ctrl Pts',(22.4660285563183,-0.0636652448434586,
3.40926951931498));
#27364=CARTESIAN_POINT('Ctrl Pts',(22.4739811956621,0.0346915369593057,
3.39866923964846));
#27365=CARTESIAN_POINT('Ctrl Pts',(22.4819338350059,0.135753204669356,3.41316675920307));
#27366=CARTESIAN_POINT('Ctrl Pts',(22.4898864743497,0.227163587879617,3.45098955584192));
#27367=CARTESIAN_POINT('Ctrl Pts',(22.4978391136936,0.318573971089878,3.48881235248077));
#27368=CARTESIAN_POINT('Ctrl Pts',(22.5057917530374,0.40033306980035,3.54996042620388));
#27369=CARTESIAN_POINT('Ctrl Pts',(22.5137443923812,0.462444730281743,3.62695759769032));
#27370=CARTESIAN_POINT('Ctrl Pts',(22.521697031725,0.524556390763143,3.70395476917678));
#27371=CARTESIAN_POINT('Ctrl Pts',(22.5296496710688,0.567020613015458,3.79680103842659));
#27372=CARTESIAN_POINT('Ctrl Pts',(22.5376023104126,0.584645549343987,3.89414467407578));
#27373=CARTESIAN_POINT('Ctrl Pts',(22.5455549497564,0.602270485672515,3.99148830972497));
#27374=CARTESIAN_POINT('Ctrl Pts',(22.5535075891002,0.595056136077256,4.09332931177355));
#27375=CARTESIAN_POINT('Ctrl Pts',(22.561460228444,0.563884587368514,4.18721625032571));
#27376=CARTESIAN_POINT('Ctrl Pts',(22.5694128677878,0.532713038659782,4.28110318887784));
#27377=CARTESIAN_POINT('Ctrl Pts',(22.5773655071316,0.477584290837583,4.36703606393356));
#27378=CARTESIAN_POINT('Ctrl Pts',(22.5853181464754,0.405238519368296,4.43450837402952));
#27379=CARTESIAN_POINT('Ctrl Pts',(22.5932707858192,0.332892747898984,4.5019806841255));
#27380=CARTESIAN_POINT('Ctrl Pts',(22.601223425163,0.24332995278257,4.55099242926169));
#27381=CARTESIAN_POINT('Ctrl Pts',(22.6091760645068,0.14750052788588,4.57555132613148));
#27382=CARTESIAN_POINT('Ctrl Pts',(22.6131689059187,0.0993867282199646,
4.58788179608141));
#27383=CARTESIAN_POINT('Ctrl Pts',(22.6171617473306,0.0496932250345643,
4.5940481472271));
#27384=CARTESIAN_POINT('Ctrl Pts',(22.6211545887425,-1.51173456864708E-7,
4.59404872180247));
#27385=CARTESIAN_POINT('Origin',(3.42660065607856,0.,4.));
#27386=CARTESIAN_POINT('',(22.7766006560786,-4.98014040841517E-7,4.41590979742004));
#27387=CARTESIAN_POINT('',(22.8,4.87367679877478E-13,4.415875));
#27388=CARTESIAN_POINT('',(3.42660065607856,4.87367679877478E-13,4.415875));
#27389=CARTESIAN_POINT('',(22.8,-0.195748955928421,4.36692555359082));
#27390=CARTESIAN_POINT('Ctrl Pts',(22.7766006560786,-4.98014040834069E-7,
4.41590979742004));
#27391=CARTESIAN_POINT('Ctrl Pts',(22.7844004373857,-0.0679170312443507,
4.41589851620688));
#27392=CARTESIAN_POINT('Ctrl Pts',(22.7922002186928,-0.135834416676695,
4.39892762624317));
#27393=CARTESIAN_POINT('Ctrl Pts',(22.8,-0.195762566582618,4.36695865185838));
#27394=CARTESIAN_POINT('Origin',(22.8,0.,4.));
#27395=CARTESIAN_POINT('Origin',(3.42660065607856,0.,4.));
#27396=CARTESIAN_POINT('',(22.4766006560785,3.63249072247605E-6,4.41584094994071));
#27397=CARTESIAN_POINT('',(22.5733993439214,-1.05822049303872E-7,4.41583910483016));
#27398=CARTESIAN_POINT('',(3.42660065607856,4.87367679877478E-13,4.415875));
#27399=CARTESIAN_POINT('Ctrl Pts',(22.4766006560785,3.63249072248342E-6,
4.41584094994071));
#27400=CARTESIAN_POINT('Ctrl Pts',(22.4810292621689,-0.0385780726118879,
4.41582919621688));
#27401=CARTESIAN_POINT('Ctrl Pts',(22.4934105076031,-0.146451497349971,
4.40094585736882));
#27402=CARTESIAN_POINT('Ctrl Pts',(22.5137443923812,-0.304292138366774,
4.30886736509782));
#27403=CARTESIAN_POINT('Ctrl Pts',(22.5376023104126,-0.415080201412036,
4.12530439950267));
#27404=CARTESIAN_POINT('Ctrl Pts',(22.561460228444,-0.424369795825249,3.91110111771763));
#27405=CARTESIAN_POINT('Ctrl Pts',(22.5853181464754,-0.329889515310188,
3.71863599132299));
#27406=CARTESIAN_POINT('Ctrl Pts',(22.6091760645068,-0.154742073939436,
3.59497211022641));
#27407=CARTESIAN_POINT('Ctrl Pts',(22.6330339825383,0.0582436639512456,
3.57034842802071));
#27408=CARTESIAN_POINT('Ctrl Pts',(22.6568919005697,0.256987911016647,3.65078654733876));
#27409=CARTESIAN_POINT('Ctrl Pts',(22.6807498186011,0.39289034562191,3.81661632308649));
#27410=CARTESIAN_POINT('Ctrl Pts',(22.7046077366325,0.432722782933869,4.02728943245291));
#27411=CARTESIAN_POINT('Ctrl Pts',(22.7284656546639,0.366738191089385,4.2312875884069));
#27412=CARTESIAN_POINT('Ctrl Pts',(22.7523235726953,0.211084664509997,4.37873330099785));
#27413=CARTESIAN_POINT('Ctrl Pts',(22.7683685731669,0.0716802821347026,
4.41560650088387));
#27414=CARTESIAN_POINT('Ctrl Pts',(22.7764609342946,0.00121612829983627,
4.41590999950663));
#27415=CARTESIAN_POINT('Ctrl Pts',(22.7766006560786,-4.98014040834069E-7,
4.41590979742004));
#27416=CARTESIAN_POINT('',(22.8,0.415641328671541,4.01393920819689));
#27417=CARTESIAN_POINT('Origin',(22.8,0.,4.));
#27418=CARTESIAN_POINT('Ctrl Pts',(22.5733993439214,-1.0582204931428E-7,
4.41583910483016));
#27419=CARTESIAN_POINT('Ctrl Pts',(22.5773591418533,-0.034498011376554,
4.41583950370926));
#27420=CARTESIAN_POINT('Ctrl Pts',(22.5892715791291,-0.138279341065089,
4.40307041914735));
#27421=CARTESIAN_POINT('Ctrl Pts',(22.6091366557487,-0.295063722636797,
4.31769517074077));
#27422=CARTESIAN_POINT('Ctrl Pts',(22.6329945737801,-0.411209141905604,
4.13747522778479));
#27423=CARTESIAN_POINT('Ctrl Pts',(22.6568524918115,-0.426804986482714,
3.92363755172126));
#27424=CARTESIAN_POINT('Ctrl Pts',(22.6807104098429,-0.33803111495158,3.72847502015617));
#27425=CARTESIAN_POINT('Ctrl Pts',(22.7045683278743,-0.16660749730952,3.59970312177549));
#27426=CARTESIAN_POINT('Ctrl Pts',(22.7284262459057,0.0455714674079685,
3.56882345794434));
#27427=CARTESIAN_POINT('Ctrl Pts',(22.7522841639372,0.246577802732478,3.64336153500176));
#27428=CARTESIAN_POINT('Ctrl Pts',(22.7761420819686,0.387346815298129,3.80514019809748));
#27429=CARTESIAN_POINT('Ctrl Pts',(22.7920473606562,0.417963038852713,3.94471011778788));
#27430=CARTESIAN_POINT('Ctrl Pts',(22.8,0.415641328671541,4.01393920819689));
#27431=CARTESIAN_POINT('Origin',(3.42660065607856,0.,4.));
#27432=CARTESIAN_POINT('',(22.1766006560786,-8.37799962078257E-6,4.41589611849309));
#27433=CARTESIAN_POINT('',(22.2733993439214,-5.11585294796223E-6,4.41590580604266));
#27434=CARTESIAN_POINT('',(3.42660065607856,4.87367679877478E-13,4.415875));
#27435=CARTESIAN_POINT('Ctrl Pts',(22.1766006560786,-8.37799962077716E-6,
4.41589611849309));
#27436=CARTESIAN_POINT('Ctrl Pts',(22.1776449506995,-0.0091027307950905,
4.41590434335565));
#27437=CARTESIAN_POINT('Ctrl Pts',(22.1866418846642,-0.0874489573854402,
4.4133870032437));
#27438=CARTESIAN_POINT('Ctrl Pts',(22.2035914579727,-0.232253957950086,
4.36612956178204));
#27439=CARTESIAN_POINT('Ctrl Pts',(22.2274493760041,-0.379286482964224,
4.21008217638027));
#27440=CARTESIAN_POINT('Ctrl Pts',(22.2513072940356,-0.433573131350875,
4.00266397632408));
#27441=CARTESIAN_POINT('Ctrl Pts',(22.275165212067,-0.381839338801546,3.79459436150246));
#27442=CARTESIAN_POINT('Ctrl Pts',(22.2990231300984,-0.236735426869051,
3.63675202040985));
#27443=CARTESIAN_POINT('Ctrl Pts',(22.3228810481298,-0.0337432544318164,
3.56773370504276));
#27444=CARTESIAN_POINT('Ctrl Pts',(22.3467389661613,0.177500062688638,3.60441627341574));
#27445=CARTESIAN_POINT('Ctrl Pts',(22.3705968841926,0.345339779804043,3.73782983856348));
#27446=CARTESIAN_POINT('Ctrl Pts',(22.3944548022241,0.428734513273282,3.93535114928888));
#27447=CARTESIAN_POINT('Ctrl Pts',(22.4183127202555,0.407291980919218,4.1486808655136));
#27448=CARTESIAN_POINT('Ctrl Pts',(22.4421706382869,0.286255462618544,4.32565405918856));
#27449=CARTESIAN_POINT('Ctrl Pts',(22.4615999502279,0.130682174689606,4.40492695636159));
#27450=CARTESIAN_POINT('Ctrl Pts',(22.4730766228251,0.0307047625933256,
4.41585030288671));
#27451=CARTESIAN_POINT('Ctrl Pts',(22.4766006560785,3.63249072248342E-6,
4.41584094994071));
#27452=CARTESIAN_POINT('Ctrl Pts',(22.2733993439214,-5.11585294797612E-6,
4.41590580604266));
#27453=CARTESIAN_POINT('Ctrl Pts',(22.2739748303838,-0.0050164638240448,
4.41590888908576));
#27454=CARTESIAN_POINT('Ctrl Pts',(22.2825029561901,-0.0792779396689182,
4.41459464077989));
#27455=CARTESIAN_POINT('Ctrl Pts',(22.2989837213402,-0.221370022215225,
4.37281103827166));
#27456=CARTESIAN_POINT('Ctrl Pts',(22.3228416393716,-0.372934645290675,
4.22116172228637));
#27457=CARTESIAN_POINT('Ctrl Pts',(22.346699557403,-0.43330658847365,4.01543234121164));
#27458=CARTESIAN_POINT('Ctrl Pts',(22.3705574754345,-0.387723268841402,
3.80592933171158));
#27459=CARTESIAN_POINT('Ctrl Pts',(22.3944153934659,-0.247331046528593,
3.64388188817752));
#27460=CARTESIAN_POINT('Ctrl Pts',(22.4182733114973,-0.0464596501027702,
3.56891502119853));
#27461=CARTESIAN_POINT('Ctrl Pts',(22.4421312295287,0.165772403721094,3.59936017830047));
#27462=CARTESIAN_POINT('Ctrl Pts',(22.4659891475602,0.337468575289321,3.7277726770023));
#27463=CARTESIAN_POINT('Ctrl Pts',(22.4898470655915,0.426644514167594,3.92275218663495));
#27464=CARTESIAN_POINT('Ctrl Pts',(22.513704983623,0.411494197867752,4.13662086224655));
#27465=CARTESIAN_POINT('Ctrl Pts',(22.5375629016544,0.295722435535401,4.31708206952049));
#27466=CARTESIAN_POINT('Ctrl Pts',(22.5574610217539,0.138855410360913,4.40292493148274));
#27467=CARTESIAN_POINT('Ctrl Pts',(22.5694065025095,0.0347856757474044,
4.41583870262252));
#27468=CARTESIAN_POINT('Ctrl Pts',(22.5733993439214,-1.0582204931428E-7,
4.41583910483016));
#27469=CARTESIAN_POINT('Origin',(3.42660065607856,0.,4.));
#27470=CARTESIAN_POINT('',(21.8766006560786,1.03078286340212E-5,4.41586151989188));
#27471=CARTESIAN_POINT('',(21.9733993439214,8.40473402259622E-6,4.41585103914036));
#27472=CARTESIAN_POINT('',(3.42660065607856,4.87367679877478E-13,4.415875));
#27473=CARTESIAN_POINT('Ctrl Pts',(21.8766006560786,1.03078286340201E-5,
4.41586151989188));
#27474=CARTESIAN_POINT('Ctrl Pts',(21.8822132785738,-0.0488795353146484,
4.415816298089));
#27475=CARTESIAN_POINT('Ctrl Pts',(21.8957785404128,-0.167079919178725,
4.39498170153279));
#27476=CARTESIAN_POINT('Ctrl Pts',(21.9172964415957,-0.326407159500644,
4.28539643168872));
#27477=CARTESIAN_POINT('Ctrl Pts',(21.9411543596271,-0.423245389017799,
4.09410684177624));
#27478=CARTESIAN_POINT('Ctrl Pts',(21.9650122776585,-0.416588591947193,
3.87980556563057));
#27479=CARTESIAN_POINT('Ctrl Pts',(21.98887019569,-0.30806453650007,3.69489510271888));
#27480=CARTESIAN_POINT('Ctrl Pts',(22.0127281137213,-0.12421031036921,3.58459109808296));
#27481=CARTESIAN_POINT('Ctrl Pts',(22.0365860317528,0.0900167200678817,
3.57586588547707));
#27482=CARTESIAN_POINT('Ctrl Pts',(22.0604439497842,0.282232210442068,3.67085301705332));
#27483=CARTESIAN_POINT('Ctrl Pts',(22.0843018678157,0.405434237512275,3.8463255517439));
#27484=CARTESIAN_POINT('Ctrl Pts',(22.108159785847,0.429496549703537,4.05937567504088));
#27485=CARTESIAN_POINT('Ctrl Pts',(22.1320177038785,0.348535256241736,4.25790682842971));
#27486=CARTESIAN_POINT('Ctrl Pts',(22.1548313272889,0.18962186617866,4.38744320371645));
#27487=CARTESIAN_POINT('Ctrl Pts',(22.1696923113557,0.0601536901409818,
4.41584170838249));
#27488=CARTESIAN_POINT('Ctrl Pts',(22.1766006560786,-8.37799962077716E-6,
4.41589611849309));
#27489=CARTESIAN_POINT('Ctrl Pts',(21.9733993439214,8.40473402260317E-6,
4.41585103914036));
#27490=CARTESIAN_POINT('Ctrl Pts',(21.9785431582582,-0.044801031555974,
4.41581845947763));
#27491=CARTESIAN_POINT('Ctrl Pts',(21.9916396119388,-0.158914563981884,
4.39744691543598));
#27492=CARTESIAN_POINT('Ctrl Pts',(22.0126887049632,-0.317860118355158,
4.29488591379237));
#27493=CARTESIAN_POINT('Ctrl Pts',(22.0365466229946,-0.420290167226249,
4.10653136780738));
#27494=CARTESIAN_POINT('Ctrl Pts',(22.060404541026,-0.419947821735935,3.89212700053744));
#27495=CARTESIAN_POINT('Ctrl Pts',(22.0842624590574,-0.316916794682727,
3.70410052003731));
#27496=CARTESIAN_POINT('Ctrl Pts',(22.1081203770888,-0.136390978688423,
3.58842952252864));
#27497=CARTESIAN_POINT('Ctrl Pts',(22.1319782951203,0.0774861468089536,
3.57339871771534));
#27498=CARTESIAN_POINT('Ctrl Pts',(22.1558362131517,0.27241579873489,3.66268354680831));
#27499=CARTESIAN_POINT('Ctrl Pts',(22.1796941311831,0.400732367405962,3.83445143701846));
#27500=CARTESIAN_POINT('Ctrl Pts',(22.2035520492145,0.431058956528623,4.04670046033727));
#27501=CARTESIAN_POINT('Ctrl Pts',(22.227409967246,0.355979888945518,4.24752994899471));
#27502=CARTESIAN_POINT('Ctrl Pts',(22.2506923988149,0.197764744804664,4.38444734931837));
#27503=CARTESIAN_POINT('Ctrl Pts',(22.26602219104,0.064235283418036,4.41586628455644));
#27504=CARTESIAN_POINT('Ctrl Pts',(22.2733993439214,-5.11585294797612E-6,
4.41590580604266));
#27505=CARTESIAN_POINT('Origin',(3.42660065607856,0.,4.));
#27506=CARTESIAN_POINT('',(21.5766006560785,-1.05752387382048E-5,4.41586434469346));
#27507=CARTESIAN_POINT('',(21.6733993439214,-1.08222664516599E-5,4.41587700699864));
#27508=CARTESIAN_POINT('',(3.42660065607856,4.87367679877478E-13,4.415875));
#27509=CARTESIAN_POINT('Ctrl Pts',(21.5766006560785,-1.05752387381843E-5,
4.41586434469346));
#27510=CARTESIAN_POINT('Ctrl Pts',(21.5788289671043,-0.0194203346498642,
4.41588296395747));
#27511=CARTESIAN_POINT('Ctrl Pts',(21.5890099174739,-0.10809016089515,4.40978779866957));
#27512=CARTESIAN_POINT('Ctrl Pts',(21.6071435071872,-0.258824259222961,
4.34785450957493));
#27513=CARTESIAN_POINT('Ctrl Pts',(21.6310014252187,-0.39385182381868,4.18131050126406));
#27514=CARTESIAN_POINT('Ctrl Pts',(21.6548593432501,-0.432571889182456,
3.97043113659525));
#27515=CARTESIAN_POINT('Ctrl Pts',(21.6787172612815,-0.365516344619441,
3.76678216446856));
#27516=CARTESIAN_POINT('Ctrl Pts',(21.702575179313,-0.209082097331647,3.62016130585559));
#27517=CARTESIAN_POINT('Ctrl Pts',(21.7264330973443,-0.00152158196427748,
3.56642135455923));
#27518=CARTESIAN_POINT('Ctrl Pts',(21.7502910153758,0.206411001640417,3.61870319251831));
#27519=CARTESIAN_POINT('Ctrl Pts',(21.7741489334072,0.363870472821225,3.76422248622317));
#27520=CARTESIAN_POINT('Ctrl Pts',(21.7980068514386,0.432353701764573,3.96739580449697));
#27521=CARTESIAN_POINT('Ctrl Pts',(21.82186476947,0.395114673548107,4.17854173669174));
#27522=CARTESIAN_POINT('Ctrl Pts',(21.8457226875014,0.261259344941517,4.3460293508861));
#27523=CARTESIAN_POINT('Ctrl Pts',(21.8639679830376,0.110037800305057,4.4094070875278));
#27524=CARTESIAN_POINT('Ctrl Pts',(21.87426063923,0.0203934810735595,4.41588037378429));
#27525=CARTESIAN_POINT('Ctrl Pts',(21.8766006560786,1.03078286340201E-5,
4.41586151989188));
#27526=CARTESIAN_POINT('Ctrl Pts',(21.6733993439214,-1.0822266451653E-5,
4.41587700699864));
#27527=CARTESIAN_POINT('Ctrl Pts',(21.6751588467887,-0.0153356749568721,
4.41589290068126));
#27528=CARTESIAN_POINT('Ctrl Pts',(21.6848709889998,-0.0999166717736498,
4.41130778913604));
#27529=CARTESIAN_POINT('Ctrl Pts',(21.7025357705547,-0.248467031045983,
4.35532645760922));
#27530=CARTESIAN_POINT('Ctrl Pts',(21.7263936885861,-0.388341045935521,
4.1928315042612));
#27531=CARTESIAN_POINT('Ctrl Pts',(21.7502516066176,-0.433255096896122,
3.98318399549658));
#27532=CARTESIAN_POINT('Ctrl Pts',(21.774109524649,-0.372226475033738,3.77764845789182));
#27533=CARTESIAN_POINT('Ctrl Pts',(21.7979674426804,-0.220178340780001,
3.62648392906691));
#27534=CARTESIAN_POINT('Ctrl Pts',(21.8218253607118,-0.0142906046679706,
3.56665425395863));
#27535=CARTESIAN_POINT('Ctrl Pts',(21.8456832787432,0.195091573553633,3.61278941785858));
#27536=CARTESIAN_POINT('Ctrl Pts',(21.8695411967747,0.356768547853618,3.75360811649661));
#27537=CARTESIAN_POINT('Ctrl Pts',(21.8933991148061,0.431205894023261,3.95467634223136));
#27538=CARTESIAN_POINT('Ctrl Pts',(21.9172570328375,0.400201653291494,4.16682743688221));
#27539=CARTESIAN_POINT('Ctrl Pts',(21.941114950869,0.271337207055788,4.33818467892719));
#27540=CARTESIAN_POINT('Ctrl Pts',(21.9598290545635,0.118211900824938,4.40773087908456));
#27541=CARTESIAN_POINT('Ctrl Pts',(21.9705905189143,0.0244769910710258,
4.41586882955141));
#27542=CARTESIAN_POINT('Ctrl Pts',(21.9733993439214,8.40473402260317E-6,
4.41585103914036));
#27543=CARTESIAN_POINT('Origin',(3.42660065607856,0.,4.));
#27544=CARTESIAN_POINT('',(21.2766006560785,8.9771325895615E-6,4.41589335210553));
#27545=CARTESIAN_POINT('',(21.3733993439214,1.06214664634743E-5,4.41588075133303));
#27546=CARTESIAN_POINT('',(3.42660065607856,4.87367679877478E-13,4.415875));
#27547=CARTESIAN_POINT('Ctrl Pts',(21.2766006560785,8.97713258955941E-6,
4.41589335210553));
#27548=CARTESIAN_POINT('Ctrl Pts',(21.2833972949786,-0.0591814269577189,
4.41583723296416));
#27549=CARTESIAN_POINT('Ctrl Pts',(21.2981465732225,-0.187680420990878,
4.38813575385326));
#27550=CARTESIAN_POINT('Ctrl Pts',(21.3208484908102,-0.346716519889314,
4.26034671465164));
#27551=CARTESIAN_POINT('Ctrl Pts',(21.3447064088417,-0.429069235164158,
4.0623886883135));
#27552=CARTESIAN_POINT('Ctrl Pts',(21.368564326873,-0.406502834830527,3.8491749282489));
#27553=CARTESIAN_POINT('Ctrl Pts',(21.3924222449045,-0.284535418465691,
3.67284200661995));
#27554=CARTESIAN_POINT('Ctrl Pts',(21.4162801629359,-0.0929913416969399,
3.5765081259772));
#27555=CARTESIAN_POINT('Ctrl Pts',(21.4401380809674,0.121291651150069,3.58372954422009));
#27556=CARTESIAN_POINT('Ctrl Pts',(21.4639959989987,0.305915531372611,3.69274042788069));
#27557=CARTESIAN_POINT('Ctrl Pts',(21.4878539170302,0.415734731202803,3.87688464650718));
#27558=CARTESIAN_POINT('Ctrl Pts',(21.5117118350615,0.423895464867194,4.09113392265755));
#27559=CARTESIAN_POINT('Ctrl Pts',(21.535569753093,0.328402210690932,4.28309847227994));
#27560=CARTESIAN_POINT('Ctrl Pts',(21.5571993600986,0.169024930905334,4.39437398220882));
#27561=CARTESIAN_POINT('Ctrl Pts',(21.5708763277605,0.0498513310028489,
4.41581651349798));
#27562=CARTESIAN_POINT('Ctrl Pts',(21.5766006560785,-1.05752387381843E-5,
4.41586434469346));
#27563=CARTESIAN_POINT('Ctrl Pts',(21.3733993439214,1.06214664634605E-5,
4.41588075133303));
#27564=CARTESIAN_POINT('Ctrl Pts',(21.379727174663,-0.0551018547626871,
4.41582358345633));
#27565=CARTESIAN_POINT('Ctrl Pts',(21.3940076447484,-0.1795281855266,4.39095386216025));
#27566=CARTESIAN_POINT('Ctrl Pts',(21.4162407541777,-0.338898428465248,
4.27044521104599));
#27567=CARTESIAN_POINT('Ctrl Pts',(21.4400986722091,-0.427045644525908,
4.07499849655415));
#27568=CARTESIAN_POINT('Ctrl Pts',(21.4639565902406,-0.410768568010174,
3.86121260673678));
#27569=CARTESIAN_POINT('Ctrl Pts',(21.4878145082719,-0.294047387504818,
3.68136401506497));
#27570=CARTESIAN_POINT('Ctrl Pts',(21.5116724263034,-0.105423611064507,
3.57943060117972));
#27571=CARTESIAN_POINT('Ctrl Pts',(21.5355303443348,0.108979109962582,3.58033786138646));
#27572=CARTESIAN_POINT('Ctrl Pts',(21.5593882623662,0.296733470072461,3.68386394585134));
#27573=CARTESIAN_POINT('Ctrl Pts',(21.5832461803976,0.411928413892185,3.86469390692879));
#27574=CARTESIAN_POINT('Ctrl Pts',(21.6071040984291,0.426395639810567,4.07860989342611));
#27575=CARTESIAN_POINT('Ctrl Pts',(21.6309620164605,0.33659751701124,4.27330361969026));
#27576=CARTESIAN_POINT('Ctrl Pts',(21.6530604316246,0.177184770587036,4.39173732935402));
#27577=CARTESIAN_POINT('Ctrl Pts',(21.6672062074449,0.0539299276789421,
4.41582106406873));
#27578=CARTESIAN_POINT('Ctrl Pts',(21.6733993439214,-1.0822266451653E-5,
4.41587700699864));
#27579=CARTESIAN_POINT('Origin',(3.42660065607856,0.,4.));
#27580=CARTESIAN_POINT('',(20.9766006560786,-4.48287659654576E-6,4.41584197426197));
#27581=CARTESIAN_POINT('',(21.0733993439214,-7.65157297119567E-6,4.41584853425778));
#27582=CARTESIAN_POINT('',(3.42660065607856,4.87367679877478E-13,4.415875));
#27583=CARTESIAN_POINT('Ctrl Pts',(20.9766006560786,-4.48287659652116E-6,
4.41584197426197));
#27584=CARTESIAN_POINT('Ctrl Pts',(20.9800129835092,-0.0297322302090305,
4.41585318364051));
#27585=CARTESIAN_POINT('Ctrl Pts',(20.9913779502836,-0.128734546054536,
4.40538471300776));
#27586=CARTESIAN_POINT('Ctrl Pts',(21.0106955564018,-0.28396276796243,4.32765515869354));
#27587=CARTESIAN_POINT('Ctrl Pts',(21.0345534744332,-0.40623841344949,4.15153583326342));
#27588=CARTESIAN_POINT('Ctrl Pts',(21.0584113924646,-0.429177699343215,
3.93836186909709));
#27589=CARTESIAN_POINT('Ctrl Pts',(21.082269310496,-0.347171348131155,3.74026010679315));
#27590=CARTESIAN_POINT('Ctrl Pts',(21.1061272285274,-0.180272145040548,
3.605671823621));
#27591=CARTESIAN_POINT('Ctrl Pts',(21.1299851465589,0.0307085077608185,
3.56750752082027));
#27592=CARTESIAN_POINT('Ctrl Pts',(21.1538430645903,0.234180094072738,3.63509941005724));
#27593=CARTESIAN_POINT('Ctrl Pts',(21.1777009826217,0.380388268371489,3.79191943321731));
#27594=CARTESIAN_POINT('Ctrl Pts',(21.2015589006531,0.433581149524578,3.99962082296209));
#27595=CARTESIAN_POINT('Ctrl Pts',(21.2254168186846,0.380751629084578,4.2074149318183));
#27596=CARTESIAN_POINT('Ctrl Pts',(21.2492747367159,0.234817963878357,4.36449043997717));
#27597=CARTESIAN_POINT('Ctrl Pts',(21.2663360158473,0.0893960873046664,
4.41308118928586));
#27598=CARTESIAN_POINT('Ctrl Pts',(21.2754446556348,0.0100763257733538,
4.41590289708112));
#27599=CARTESIAN_POINT('Ctrl Pts',(21.2766006560785,8.97713258955941E-6,
4.41589335210553));
#27600=CARTESIAN_POINT('Ctrl Pts',(21.0733993439214,-7.65157297121996E-6,
4.41584853425778));
#27601=CARTESIAN_POINT('Ctrl Pts',(21.0763428631935,-0.0256500457845501,
4.41586537097631));
#27602=CARTESIAN_POINT('Ctrl Pts',(21.0872390218095,-0.120560449820324,
4.40722571769055));
#27603=CARTESIAN_POINT('Ctrl Pts',(21.1060878197692,-0.274189543318984,
4.33587624407661));
#27604=CARTESIAN_POINT('Ctrl Pts',(21.1299457378007,-0.401599180171465,
4.16343456021562));
#27605=CARTESIAN_POINT('Ctrl Pts',(21.1538036558321,-0.430806878168669,
3.95102867450389));
#27606=CARTESIAN_POINT('Ctrl Pts',(21.1776615738635,-0.354670559489406,
3.75059761183336));
#27607=CARTESIAN_POINT('Ctrl Pts',(21.2015194918949,-0.191807627993766,
3.61115222665144));
#27608=CARTESIAN_POINT('Ctrl Pts',(21.2253774099264,0.0179574932869785,
3.56679071405539));
#27609=CARTESIAN_POINT('Ctrl Pts',(21.2492353279577,0.223331518303719,3.62836067225603));
#27610=CARTESIAN_POINT('Ctrl Pts',(21.2730932459892,0.374094903668402,3.78080656934254));
#27611=CARTESIAN_POINT('Ctrl Pts',(21.2969511640206,0.433381894944723,3.98685123093373));
#27612=CARTESIAN_POINT('Ctrl Pts',(21.320809082052,0.386695207821707,4.19611112472705));
#27613=CARTESIAN_POINT('Ctrl Pts',(21.3446670000834,0.245451009020076,4.35741650656472));
#27614=CARTESIAN_POINT('Ctrl Pts',(21.3621970873732,0.0975684711839555,
4.41172139589413));
#27615=CARTESIAN_POINT('Ctrl Pts',(21.3717745353192,0.014161952170494,4.41589543043265));
#27616=CARTESIAN_POINT('Ctrl Pts',(21.3733993439214,1.06214664634605E-5,
4.41588075133303));
#27617=CARTESIAN_POINT('Origin',(3.42660065607856,0.,4.));
#27618=CARTESIAN_POINT('',(20.6766006560786,1.29204965968245E-6,4.41591114679826));
#27619=CARTESIAN_POINT('',(20.7733993439214,3.9567662055099E-6,4.41590779860895));
#27620=CARTESIAN_POINT('',(3.42660065607856,4.87367679877478E-13,4.415875));
#27621=CARTESIAN_POINT('Ctrl Pts',(20.6766006560786,1.29076178055295E-6,
4.41591111076812));
#27622=CARTESIAN_POINT('Ctrl Pts',(20.6766286720397,-0.000242659277546582,
4.41591112051333));
#27623=CARTESIAN_POINT('Ctrl Pts',(20.6846093273446,-0.0697345275278937,
4.41585145172406));
#27624=CARTESIAN_POINT('Ctrl Pts',(20.7005426219933,-0.208420567790133,
4.38020336888205));
#27625=CARTESIAN_POINT('Ctrl Pts',(20.7244005400248,-0.365106210756856,
4.23385701605743));
#27626=CARTESIAN_POINT('Ctrl Pts',(20.7482584580562,-0.432520392530856,
4.03032528343114));
#27627=CARTESIAN_POINT('Ctrl Pts',(20.7721163760876,-0.394167874571092,
3.81937870627435));
#27628=CARTESIAN_POINT('Ctrl Pts',(20.795974294119,-0.259432524437891,3.65259868360638));
#27629=CARTESIAN_POINT('Ctrl Pts',(20.8198322121504,-0.0612578225112809,
3.57076788979259));
#27630=CARTESIAN_POINT('Ctrl Pts',(20.8436901301819,0.151895538690754,3.5938959627232));
#27631=CARTESIAN_POINT('Ctrl Pts',(20.8675480482132,0.327906592802717,3.71632757520176));
#27632=CARTESIAN_POINT('Ctrl Pts',(20.8914059662447,0.423735399567132,3.90812480123879));
#27633=CARTESIAN_POINT('Ctrl Pts',(20.9152638842761,0.415949440063929,4.12238802732943));
#27634=CARTESIAN_POINT('Ctrl Pts',(20.9391218023075,0.30645246920106,4.30672404095661));
#27635=CARTESIAN_POINT('Ctrl Pts',(20.9595673929083,0.148398440326279,4.40042000858165));
#27636=CARTESIAN_POINT('Ctrl Pts',(20.9720603441653,0.0395501167658222,
4.4158270594931));
#27637=CARTESIAN_POINT('Ctrl Pts',(20.9766006560786,-4.48287659652116E-6,
4.41584197426197));
#27638=CARTESIAN_POINT('Ctrl Pts',(20.7733993439214,3.95676620551077E-6,
4.41590779860895));
#27639=CARTESIAN_POINT('Ctrl Pts',(20.7809111910678,-0.0654084660523611,
4.41587519962517));
#27640=CARTESIAN_POINT('Ctrl Pts',(20.7963756775582,-0.200102595337945,
4.3835597345012));
#27641=CARTESIAN_POINT('Ctrl Pts',(20.8197928033922,-0.358062019934396,
4.24450842127602));
#27642=CARTESIAN_POINT('Ctrl Pts',(20.8436507214237,-0.431438726014498,
4.04305074550709));
#27643=CARTESIAN_POINT('Ctrl Pts',(20.867508639455,-0.399316990859146,3.83106596928302));
#27644=CARTESIAN_POINT('Ctrl Pts',(20.8913665574865,-0.269551332195825,
3.66039017609669));
#27645=CARTESIAN_POINT('Ctrl Pts',(20.9152244755179,-0.0738730526583281,
3.57275822989076));
#27646=CARTESIAN_POINT('Ctrl Pts',(20.9390823935493,0.139869212314499,3.58959853735383));
#27647=CARTESIAN_POINT('Ctrl Pts',(20.9629403115807,0.319409638666883,3.70679317993256));
#27648=CARTESIAN_POINT('Ctrl Pts',(20.9867982296122,0.420845711130686,3.8956848776653));
#27649=CARTESIAN_POINT('Ctrl Pts',(21.0106561476436,0.419373541863394,4.11008446384341));
#27650=CARTESIAN_POINT('Ctrl Pts',(21.034514065675,0.315353119032788,4.29756540021079));
#27651=CARTESIAN_POINT('Ctrl Pts',(21.0554284644342,0.156567902793621,4.39812991232556));
#27652=CARTESIAN_POINT('Ctrl Pts',(21.0683902238497,0.0436291721249729,
4.41581988245125));
#27653=CARTESIAN_POINT('Ctrl Pts',(21.0733993439214,-7.65157297121996E-6,
4.41584853425778));
#27654=CARTESIAN_POINT('Origin',(3.42660065607856,0.,4.));
#27655=CARTESIAN_POINT('',(20.3766006560786,0.000383027521040961,4.41597069455794));
#27656=CARTESIAN_POINT('',(20.4733993439214,0.000101608071013781,4.41586489633469));
#27657=CARTESIAN_POINT('',(3.42660065607856,4.87367679877478E-13,4.415875));
#27658=CARTESIAN_POINT('Ctrl Pts',(20.3766006560786,0.000383027521040954,
4.41597069455794));
#27659=CARTESIAN_POINT('Ctrl Pts',(20.3891496392578,-0.108893832387875,
4.41487837761012));
#27660=CARTESIAN_POINT('Ctrl Pts',(20.4176039011246,-0.35839559572325,4.31454223548297));
#27661=CARTESIAN_POINT('Ctrl Pts',(20.4540108023354,-0.457800032585507,
3.97025345815189));
#27662=CARTESIAN_POINT('Ctrl Pts',(20.4858213597105,-0.325993724402262,
3.71529210935379));
#27663=CARTESIAN_POINT('Ctrl Pts',(20.509679277742,-0.15096738523986,3.59329490328468));
#27664=CARTESIAN_POINT('Ctrl Pts',(20.5335371957734,0.0630371972956549,
3.57102347342756));
#27665=CARTESIAN_POINT('Ctrl Pts',(20.5573951138048,0.260511246441404,3.65349437971329));
#27666=CARTESIAN_POINT('Ctrl Pts',(20.5812530318362,0.394877283734959,3.82077798440408));
#27667=CARTESIAN_POINT('Ctrl Pts',(20.6051109498677,0.432370081305563,4.03184236506754));
#27668=CARTESIAN_POINT('Ctrl Pts',(20.6289688678991,0.364303478986858,4.23514367899931));
#27669=CARTESIAN_POINT('Ctrl Pts',(20.6527987699694,0.207251017164088,4.38076243960928));
#27670=CARTESIAN_POINT('Ctrl Pts',(20.6686760326959,0.0690052481014253,
4.41590835422812));
#27671=CARTESIAN_POINT('Ctrl Pts',(20.6766006560786,1.29076178055295E-6,
4.41591111076812));
#27672=CARTESIAN_POINT('Ctrl Pts',(20.4733993439214,0.000101608071013788,
4.4158648963347));
#27673=CARTESIAN_POINT('Ctrl Pts',(20.4775268795984,-0.0359150725839473,
4.41584626969953));
#27674=CARTESIAN_POINT('Ctrl Pts',(20.4896070546192,-0.141401612166324,
4.40227446254147));
#27675=CARTESIAN_POINT('Ctrl Pts',(20.5096398689838,-0.298255971346869,
4.31460392554555));
#27676=CARTESIAN_POINT('Ctrl Pts',(20.5334977870152,-0.412709509332759,
4.13311446574462));
#27677=CARTESIAN_POINT('Ctrl Pts',(20.5573557050466,-0.425936384696969,
3.91915434697803));
#27678=CARTESIAN_POINT('Ctrl Pts',(20.581213623078,-0.335173342752607,3.72492109335083));
#27679=CARTESIAN_POINT('Ctrl Pts',(20.6050715411095,-0.162364888615448,
3.59797442377207));
#27680=CARTESIAN_POINT('Ctrl Pts',(20.6289294591408,0.0501004451364318,
3.56932214892951));
#27681=CARTESIAN_POINT('Ctrl Pts',(20.6527873771723,0.250339089241223,3.64598859455508));
#27682=CARTESIAN_POINT('Ctrl Pts',(20.6766452952037,0.389350172549011,3.80921715950176));
#27683=CARTESIAN_POINT('Ctrl Pts',(20.7005032132352,0.433161330121289,4.01909908002448));
#27684=CARTESIAN_POINT('Ctrl Pts',(20.7243611312665,0.371049143609512,4.22430982617278));
#27685=CARTESIAN_POINT('Ctrl Pts',(20.748219049298,0.218207240773441,4.37467120177868));
#27686=CARTESIAN_POINT('Ctrl Pts',(20.7645651201829,0.0769305199015265,
4.41491906931248));
#27687=CARTESIAN_POINT('Ctrl Pts',(20.772958551724,0.00384233167249433,
4.41590971150433));
#27688=CARTESIAN_POINT('Ctrl Pts',(20.7733993439214,3.95676620551077E-6,
4.41590779860895));
#27689=CARTESIAN_POINT('Origin',(3.42660065607856,0.,4.));
#27690=CARTESIAN_POINT('',(20.0766006560786,-0.000186622634748148,4.41645953600834));
#27691=CARTESIAN_POINT('',(20.1733993439214,-0.000111611226006447,4.41653056081536));
#27692=CARTESIAN_POINT('',(3.42660065607856,4.87367679877478E-13,4.415875));
#27693=CARTESIAN_POINT('Ctrl Pts',(20.0766006560786,-0.000186622634748109,
4.41645953600834));
#27694=CARTESIAN_POINT('Ctrl Pts',(20.0778126884445,-0.0107019642254321,
4.4165186149328));
#27695=CARTESIAN_POINT('Ctrl Pts',(20.0949299994981,-0.159149739060163,
4.41138240526969));
#27696=CARTESIAN_POINT('Ctrl Pts',(20.1279525892393,-0.432744382500041,
4.23375285658289));
#27697=CARTESIAN_POINT('Ctrl Pts',(20.1756684253021,-0.430649333670284,
3.76246031529274));
#27698=CARTESIAN_POINT('Ctrl Pts',(20.223384261365,-0.033136228617316,3.50924504180455));
#27699=CARTESIAN_POINT('Ctrl Pts',(20.2711000974278,0.394908089060633,3.70680919012016));
#27700=CARTESIAN_POINT('Ctrl Pts',(20.3188159334906,0.460110046434968,4.17340395051402));
#27701=CARTESIAN_POINT('Ctrl Pts',(20.3539827863742,0.197028357007358,4.40022211154544));
#27702=CARTESIAN_POINT('Ctrl Pts',(20.3732443605702,0.0296097328916507,
4.416262840815));
#27703=CARTESIAN_POINT('Ctrl Pts',(20.3766006560786,0.000383027521040954,
4.41597069455794));
#27704=CARTESIAN_POINT('Ctrl Pts',(20.1733993439214,-0.000111611226006447,
4.41653056081536));
#27705=CARTESIAN_POINT('Ctrl Pts',(20.1741425681289,-0.00655727229825777,
4.41655465488103));
#27706=CARTESIAN_POINT('Ctrl Pts',(20.190791071024,-0.150919726673813,4.41348743992374));
#27707=CARTESIAN_POINT('Ctrl Pts',(20.2233448526067,-0.425711472830213,
4.24633918020534));
#27708=CARTESIAN_POINT('Ctrl Pts',(20.2710606886696,-0.437384262562023,
3.77535541015343));
#27709=CARTESIAN_POINT('Ctrl Pts',(20.3187765247324,-0.0477164433392854,
3.51022640082505));
#27710=CARTESIAN_POINT('Ctrl Pts',(20.3664923607953,0.386374384143037,3.69571627142296));
#27711=CARTESIAN_POINT('Ctrl Pts',(20.4062555575143,0.45143962727185,4.08165775845481));
#27712=CARTESIAN_POINT('Ctrl Pts',(20.4380661148895,0.291471375703242,4.31996082336987));
#27713=CARTESIAN_POINT('Ctrl Pts',(20.4577964972439,0.136183087716603,4.40372206768731));
#27714=CARTESIAN_POINT('Ctrl Pts',(20.4695742402546,0.0334792813416625,
4.41588215816259));
#27715=CARTESIAN_POINT('Ctrl Pts',(20.4733993439214,0.000101608071013788,
4.4158648963347));
#27716=CARTESIAN_POINT('Origin',(3.42660065607856,0.,4.));
#27717=CARTESIAN_POINT('',(19.7766006560786,-0.000280998963924209,4.41539029291088));
#27718=CARTESIAN_POINT('',(19.8733993439214,-0.000322938566065189,4.41548189938477));
#27719=CARTESIAN_POINT('',(3.42660065607856,4.87367679877478E-13,4.415875));
#27720=CARTESIAN_POINT('Ctrl Pts',(19.7766006560786,-0.000280998963924181,
4.41539029291088));
#27721=CARTESIAN_POINT('Ctrl Pts',(19.7823810163188,-0.0507615353771658,
4.41570272077311));
#27722=CARTESIAN_POINT('Ctrl Pts',(19.8040666552467,-0.23976299482565,4.3837755623668));
#27723=CARTESIAN_POINT('Ctrl Pts',(19.8416575728622,-0.481212499922896,
4.10168523844358));
#27724=CARTESIAN_POINT('Ctrl Pts',(19.8893734089251,-0.345789702982467,
3.65023692191923));
#27725=CARTESIAN_POINT('Ctrl Pts',(19.9370892449879,0.107175910646637,3.51998011832295));
#27726=CARTESIAN_POINT('Ctrl Pts',(19.9848050810508,0.461722480014006,3.83053541934297));
#27727=CARTESIAN_POINT('Ctrl Pts',(20.0313088847476,0.394022427012164,4.28486673161383));
#27728=CARTESIAN_POINT('Ctrl Pts',(20.0619074097569,0.127288937001902,4.4157433330307));
#27729=CARTESIAN_POINT('Ctrl Pts',(20.0766006560786,-0.000186622634748109,
4.41645953600834));
#27730=CARTESIAN_POINT('Ctrl Pts',(19.8733993439214,-0.000322938566065196,
4.41548189938477));
#27731=CARTESIAN_POINT('Ctrl Pts',(19.8787108960032,-0.0466836533228258,
4.41581668875846));
#27732=CARTESIAN_POINT('Ctrl Pts',(19.8999277267727,-0.231469429366377,
4.38724295332581));
#27733=CARTESIAN_POINT('Ctrl Pts',(19.9370498362297,-0.47800980043334,4.11581244897344));
#27734=CARTESIAN_POINT('Ctrl Pts',(19.9847656722926,-0.355939225796451,
3.66057517601247));
#27735=CARTESIAN_POINT('Ctrl Pts',(20.0324815083554,0.0929888682922082,
3.51702731322357));
#27736=CARTESIAN_POINT('Ctrl Pts',(20.0801973444182,0.456536973876988,3.81701888067549));
#27737=CARTESIAN_POINT('Ctrl Pts',(20.1271699562736,0.401683300383188,4.27772103607547));
#27738=CARTESIAN_POINT('Ctrl Pts',(20.1582372894413,0.131382308576697,4.41603903277767));
#27739=CARTESIAN_POINT('Ctrl Pts',(20.1733993439214,-0.000111611226006447,
4.41653056081536));
#27740=CARTESIAN_POINT('Origin',(3.42660065607856,0.,4.));
#27741=CARTESIAN_POINT('',(19.4766006560786,0.000302289446139524,4.41543216566181));
#27742=CARTESIAN_POINT('',(19.5733993439214,0.000255464646300079,4.41534829948978));
#27743=CARTESIAN_POINT('',(3.42660065607856,4.87367679877478E-13,4.415875));
#27744=CARTESIAN_POINT('Ctrl Pts',(19.4766006560786,0.000302289446139546,
4.41543216566181));
#27745=CARTESIAN_POINT('Ctrl Pts',(19.4869493441932,-0.0900510892866153,
4.41482666801407));
#27746=CARTESIAN_POINT('Ctrl Pts',(19.5132033109954,-0.320168095705801,
4.3413809155508));
#27747=CARTESIAN_POINT('Ctrl Pts',(19.5553625564852,-0.490312813065352,
3.96128857502183));
#27748=CARTESIAN_POINT('Ctrl Pts',(19.603078392548,-0.232620797759261,3.56664935826393));
#27749=CARTESIAN_POINT('Ctrl Pts',(19.6507942286109,0.238690449241969,3.56996267500769));
#27750=CARTESIAN_POINT('Ctrl Pts',(19.6985100646737,0.490808633485035,3.96818593857384));
#27751=CARTESIAN_POINT('Ctrl Pts',(19.7404455404963,0.316268156276861,4.34384396940031));
#27752=CARTESIAN_POINT('Ctrl Pts',(19.7664757376312,0.0881410531427697,
4.41484304213512));
#27753=CARTESIAN_POINT('Ctrl Pts',(19.7766006560786,-0.000280998963924181,
4.41539029291088));
#27754=CARTESIAN_POINT('Ctrl Pts',(19.5733993439214,0.000255464646300094,
4.41534829948978));
#27755=CARTESIAN_POINT('Ctrl Pts',(19.5832792238775,-0.0860485087386658,
4.41486588036018));
#27756=CARTESIAN_POINT('Ctrl Pts',(19.6090643825213,-0.311990568344336,
4.34649332259355));
#27757=CARTESIAN_POINT('Ctrl Pts',(19.6507548198527,-0.491240257057309,
3.97574594767572));
#27758=CARTESIAN_POINT('Ctrl Pts',(19.6984706559155,-0.245282818621706,
3.57368850533185));
#27759=CARTESIAN_POINT('Ctrl Pts',(19.7461864919783,0.225921452997342,3.56311925573479));
#27760=CARTESIAN_POINT('Ctrl Pts',(19.7939023280412,0.489658867576397,3.95374471702426));
#27761=CARTESIAN_POINT('Ctrl Pts',(19.8363066120222,0.324430886710512,4.33863507066385));
#27762=CARTESIAN_POINT('Ctrl Pts',(19.8628056173156,0.0921420753912029,
4.4148141723173));
#27763=CARTESIAN_POINT('Ctrl Pts',(19.8733993439214,-0.000322938566065196,
4.41548189938477));
#27764=CARTESIAN_POINT('Origin',(3.42660065607856,0.,4.));
#27765=CARTESIAN_POINT('',(19.1766006560786,0.000155842099650094,4.41649089206047));
#27766=CARTESIAN_POINT('',(19.2733993439214,0.000220989830587742,4.4164164649367));
#27767=CARTESIAN_POINT('',(3.42660065607856,4.87367679877478E-13,4.415875));
#27768=CARTESIAN_POINT('Ctrl Pts',(19.1766006560786,0.000155842099650088,
4.41649089206047));
#27769=CARTESIAN_POINT('Ctrl Pts',(19.1915176720675,-0.129233580897558,
4.41587069825202));
#27770=CARTESIAN_POINT('Ctrl Pts',(19.2223399667441,-0.397695790553126,
4.28149179527637));
#27771=CARTESIAN_POINT('Ctrl Pts',(19.2690675401082,-0.459293044881286,
3.82405931712685));
#27772=CARTESIAN_POINT('Ctrl Pts',(19.316783376171,-0.100417177000157,3.51852142809106));
#27773=CARTESIAN_POINT('Ctrl Pts',(19.3644992122339,0.350673329058588,3.65513271950473));
#27774=CARTESIAN_POINT('Ctrl Pts',(19.4122150482967,0.479735122332443,4.10844094226069));
#27775=CARTESIAN_POINT('Ctrl Pts',(19.4495821962449,0.235804435834584,4.38544967282755));
#27776=CARTESIAN_POINT('Ctrl Pts',(19.4710440655056,0.0488163355692654,
4.4157572795781));
#27777=CARTESIAN_POINT('Ctrl Pts',(19.4766006560786,0.000302289446139546,
4.41543216566181));
#27778=CARTESIAN_POINT('Ctrl Pts',(19.2733993439214,0.000220989830587761,
4.4164164649367));
#27779=CARTESIAN_POINT('Ctrl Pts',(19.2878475517519,-0.125161313229646,
4.41561068768233));
#27780=CARTESIAN_POINT('Ctrl Pts',(19.31820103827,-0.389985711500173,4.28851341748863));
#27781=CARTESIAN_POINT('Ctrl Pts',(19.3644598034757,-0.464275578741542,
3.8376626582024));
#27782=CARTESIAN_POINT('Ctrl Pts',(19.4121756395385,-0.114554038379521,
3.52168776344319));
#27783=CARTESIAN_POINT('Ctrl Pts',(19.4598914756013,0.340364234683876,3.64495435060606));
#27784=CARTESIAN_POINT('Ctrl Pts',(19.5076073116642,0.482720800247919,4.09426482953845));
#27785=CARTESIAN_POINT('Ctrl Pts',(19.5454432677708,0.244097666198316,4.38190156491584));
#27786=CARTESIAN_POINT('Ctrl Pts',(19.5673739451899,0.0528892875329133,
4.41564251031262));
#27787=CARTESIAN_POINT('Ctrl Pts',(19.5733993439214,0.000255464646300094,
4.41534829948978));
#27788=CARTESIAN_POINT('Origin',(3.42660065607856,0.,4.));
#27789=CARTESIAN_POINT('',(18.8766006560785,-0.00038196507782994,4.41590683121974));
#27790=CARTESIAN_POINT('',(18.9733993439214,-0.000368287616214491,4.41603142687637));
#27791=CARTESIAN_POINT('',(3.42660065607856,4.87367679877478E-13,4.415875));
#27792=CARTESIAN_POINT('Ctrl Pts',(18.8766006560785,-0.000381965077829925,
4.41590683121974));
#27793=CARTESIAN_POINT('Ctrl Pts',(18.8801807212542,-0.0315488007868432,
4.41619587167324));
#27794=CARTESIAN_POINT('Ctrl Pts',(18.8996660651174,-0.200861076696893,
4.39874895857547));
#27795=CARTESIAN_POINT('Ctrl Pts',(18.9350566876684,-0.462607878309702,
4.16703046362027));
#27796=CARTESIAN_POINT('Ctrl Pts',(18.9827725237311,-0.39069124519864,3.70122654773242));
#27797=CARTESIAN_POINT('Ctrl Pts',(19.030488359794,0.0400031699426168,3.50979089028978));
#27798=CARTESIAN_POINT('Ctrl Pts',(19.0782041958568,0.433962058584907,3.76852180111673));
#27799=CARTESIAN_POINT('Ctrl Pts',(19.1259200319197,0.429406911488226,4.23982270375453));
#27800=CARTESIAN_POINT('Ctrl Pts',(19.1587188519936,0.155221332864305,4.41240136130926));
#27801=CARTESIAN_POINT('Ctrl Pts',(19.1756123933799,0.00872798149047904,
4.41653198033223));
#27802=CARTESIAN_POINT('Ctrl Pts',(19.1766006560786,0.000155842099650088,
4.41649089206047));
#27803=CARTESIAN_POINT('Ctrl Pts',(18.9733993439214,-0.000368287616214533,
4.41603142687637));
#27804=CARTESIAN_POINT('Ctrl Pts',(18.9765106009386,-0.0274330213022572,
4.4162811262788));
#27805=CARTESIAN_POINT('Ctrl Pts',(18.9955271366434,-0.192586232161443,
4.40152565608163));
#27806=CARTESIAN_POINT('Ctrl Pts',(19.0304489510358,-0.457487847288108,
4.18058265263639));
#27807=CARTESIAN_POINT('Ctrl Pts',(19.0781647870987,-0.399321187381313,
3.71286272589862));
#27808=CARTESIAN_POINT('Ctrl Pts',(19.1258806231614,0.0255482632835279,
3.50882537619781));
#27809=CARTESIAN_POINT('Ctrl Pts',(19.1735964592243,0.426956350589889,3.75584124112414));
#27810=CARTESIAN_POINT('Ctrl Pts',(19.2213122952871,0.436283851722622,4.22707185138688));
#27811=CARTESIAN_POINT('Ctrl Pts',(19.2545799235195,0.163455264474221,4.41023200720537));
#27812=CARTESIAN_POINT('Ctrl Pts',(19.2719422730642,0.0128655269200745,
4.41649772584937));
#27813=CARTESIAN_POINT('Ctrl Pts',(19.2733993439214,0.000220989830587761,
4.4164164649367));
#27814=CARTESIAN_POINT('Origin',(3.42660065607856,0.,4.));
#27815=CARTESIAN_POINT('',(18.5766006560786,2.82854505807383E-5,4.41518799822097));
#27816=CARTESIAN_POINT('',(18.6733993439214,-3.94222854199766E-5,4.41518963037823));
#27817=CARTESIAN_POINT('',(3.42660065607856,4.87367679877478E-13,4.415875));
#27818=CARTESIAN_POINT('Ctrl Pts',(18.5766006560786,2.82854505807215E-5,
4.41518799822097));
#27819=CARTESIAN_POINT('Ctrl Pts',(18.5847490491285,-0.0712192880865648,
4.41514491699706));
#27820=CARTESIAN_POINT('Ctrl Pts',(18.6088027208661,-0.281596950705947,
4.36382162423513));
#27821=CARTESIAN_POINT('Ctrl Pts',(18.6487616712913,-0.49096944006335,4.0292272779409));
#27822=CARTESIAN_POINT('Ctrl Pts',(18.6964775073541,-0.290120809601049,
3.60284116440841));
#27823=CARTESIAN_POINT('Ctrl Pts',(18.744193343417,0.177150224400508,3.54117212067402));
#27824=CARTESIAN_POINT('Ctrl Pts',(18.7919091794797,0.481741481528227,3.90085177849878));
#27825=CARTESIAN_POINT('Ctrl Pts',(18.836044950367,0.354281053487698,4.31776308733785));
#27826=CARTESIAN_POINT('Ctrl Pts',(18.8642754425666,0.106917172161326,4.4149117417093));
#27827=CARTESIAN_POINT('Ctrl Pts',(18.8766006560785,-0.000381965077829925,
4.41590683121974));
#27828=CARTESIAN_POINT('Ctrl Pts',(18.6733993439214,-3.94222854199489E-5,
4.41518963037823));
#27829=CARTESIAN_POINT('Ctrl Pts',(18.6810789288129,-0.0671871929144198,
4.41524623173262));
#27830=CARTESIAN_POINT('Ctrl Pts',(18.704663792392,-0.273330541024821,4.36810584919535));
#27831=CARTESIAN_POINT('Ctrl Pts',(18.7441539346588,-0.489895661254576,
4.0436745456279));
#27832=CARTESIAN_POINT('Ctrl Pts',(18.7918697707216,-0.301692008317894,
3.6115580391236));
#27833=CARTESIAN_POINT('Ctrl Pts',(18.8395856067845,0.163560057986223,3.53615376224111));
#27834=CARTESIAN_POINT('Ctrl Pts',(18.8873014428472,0.478612406344963,3.88670662268212));
#27835=CARTESIAN_POINT('Ctrl Pts',(18.9319060218929,0.362263203066427,4.31165738429376));
#27836=CARTESIAN_POINT('Ctrl Pts',(18.960605322251,0.110926532249199,4.41500462017153));
#27837=CARTESIAN_POINT('Ctrl Pts',(18.9733993439214,-0.000368287616214533,
4.41603142687637));
#27838=CARTESIAN_POINT('Origin',(3.42660065607856,0.,4.));
#27839=CARTESIAN_POINT('',(18.2766006560786,0.000371443240938316,4.41601098728712));
#27840=CARTESIAN_POINT('',(18.3733993439214,0.000382963303967143,4.41588626824893));
#27841=CARTESIAN_POINT('',(3.42660065607856,4.87367679877478E-13,4.415875));
#27842=CARTESIAN_POINT('Ctrl Pts',(18.2766006560785,0.000371443240938293,
4.41601098728712));
#27843=CARTESIAN_POINT('Ctrl Pts',(18.2893173770028,-0.110264925490287,
4.41498710445335));
#27844=CARTESIAN_POINT('Ctrl Pts',(18.3179393766147,-0.360950442388199,
4.31267773405576));
#27845=CARTESIAN_POINT('Ctrl Pts',(18.3624666549143,-0.479157019140895,
3.88903254594255));
#27846=CARTESIAN_POINT('Ctrl Pts',(18.4101824909771,-0.165810997523729,
3.5369536330429));
#27847=CARTESIAN_POINT('Ctrl Pts',(18.4578983270399,0.299801814449608,3.61009732380414));
#27848=CARTESIAN_POINT('Ctrl Pts',(18.5056141631028,0.49010200717001,4.04129464153984));
#27849=CARTESIAN_POINT('Ctrl Pts',(18.5451816061157,0.274694351318236,4.36741107590602));
#27850=CARTESIAN_POINT('Ctrl Pts',(18.5688437704409,0.0678526130816757,
4.41522900951301));
#27851=CARTESIAN_POINT('Ctrl Pts',(18.5766006560786,2.82854505807215E-5,
4.41518799822097));
#27852=CARTESIAN_POINT('Ctrl Pts',(18.3733993439214,0.000382963303967157,
4.41588626824893));
#27853=CARTESIAN_POINT('Ctrl Pts',(18.3856472566872,-0.106256708375174,
4.41489942083623));
#27854=CARTESIAN_POINT('Ctrl Pts',(18.4138004481407,-0.352960303644862,
4.31875095920395));
#27855=CARTESIAN_POINT('Ctrl Pts',(18.4578589182817,-0.482217355384067,
3.90319273261591));
#27856=CARTESIAN_POINT('Ctrl Pts',(18.5055747543446,-0.179376629827252,
3.54203793877243));
#27857=CARTESIAN_POINT('Ctrl Pts',(18.5532905904074,0.288188414964166,3.60143675240633));
#27858=CARTESIAN_POINT('Ctrl Pts',(18.6010064264702,0.491105603945206,4.02684232898929));
#27859=CARTESIAN_POINT('Ctrl Pts',(18.6410426776416,0.282958802096416,4.36309886994028));
#27860=CARTESIAN_POINT('Ctrl Pts',(18.6651736501253,0.0718833454275778,
4.41512900400112));
#27861=CARTESIAN_POINT('Ctrl Pts',(18.6733993439214,-3.94222854199489E-5,
4.41518963037823));
#27862=CARTESIAN_POINT('Origin',(3.42660065607856,0.,4.));
#27863=CARTESIAN_POINT('',(17.9766006560786,-0.000210814279110197,4.41643020456723));
#27864=CARTESIAN_POINT('',(18.0733993439214,-0.000144384975211464,4.41650095473263));
#27865=CARTESIAN_POINT('',(3.42660065607856,4.87367679877478E-13,4.415875));
#27866=CARTESIAN_POINT('Ctrl Pts',(17.9766006560786,-0.000210814279110157,
4.41643020456723));
#27867=CARTESIAN_POINT('Ctrl Pts',(17.9779804261896,-0.0121834889824064,
4.41650424974197));
#27868=CARTESIAN_POINT('Ctrl Pts',(17.9952654749882,-0.162096873242269,
4.41059855206721));
#27869=CARTESIAN_POINT('Ctrl Pts',(18.0284558024744,-0.435175833605105,
4.22918817311999));
#27870=CARTESIAN_POINT('Ctrl Pts',(18.0761716385373,-0.428137176707308,
3.75791781814212));
#27871=CARTESIAN_POINT('Ctrl Pts',(18.1238874746,-0.0279335627019553,3.5089552556775));
#27872=CARTESIAN_POINT('Ctrl Pts',(18.1716033106629,0.397921871745719,3.71092663761881));
#27873=CARTESIAN_POINT('Ctrl Pts',(18.2193191467257,0.458359528554279,4.17835853620019));
#27874=CARTESIAN_POINT('Ctrl Pts',(18.2543182618643,0.193950155243433,4.40107745006558));
#27875=CARTESIAN_POINT('Ctrl Pts',(18.2734120983152,0.0281121206155762,
4.41626771302466));
#27876=CARTESIAN_POINT('Ctrl Pts',(18.2766006560785,0.000371443240938293,
4.41601098728712));
#27877=CARTESIAN_POINT('Ctrl Pts',(18.0733993439214,-0.000144384975211439,
4.41650095473263));
#27878=CARTESIAN_POINT('Ctrl Pts',(18.0743103058739,-0.00804551399413891,
4.41653639380418));
#27879=CARTESIAN_POINT('Ctrl Pts',(18.0911265465141,-0.153864670001157,
4.41274680364665));
#27880=CARTESIAN_POINT('Ctrl Pts',(18.1238480658419,-0.428237044548737,
4.24190547436581));
#27881=CARTESIAN_POINT('Ctrl Pts',(18.1715639019047,-0.435081213444543,
3.7706322547532));
#27882=CARTESIAN_POINT('Ctrl Pts',(18.2192797379675,-0.0423836094492617,
3.50999096487715));
#27883=CARTESIAN_POINT('Ctrl Pts',(18.2669955740304,0.389235515258945,3.69933251171255));
#27884=CARTESIAN_POINT('Ctrl Pts',(18.3147114100932,0.463413677146622,4.16478163940629));
#27885=CARTESIAN_POINT('Ctrl Pts',(18.3501793333902,0.202226156869028,4.39827758107438));
#27886=CARTESIAN_POINT('Ctrl Pts',(18.3697419779996,0.0322267809866215,
4.41618095209965));
#27887=CARTESIAN_POINT('Ctrl Pts',(18.3733993439214,0.000382963303967157,
4.41588626824893));
#27888=CARTESIAN_POINT('Origin',(3.42660065607856,0.,4.));
#27889=CARTESIAN_POINT('',(17.6766006560786,-0.000263771022561219,4.41536107794487));
#27890=CARTESIAN_POINT('',(17.7733993439214,-0.000309142357869163,4.41544738986064));
#27891=CARTESIAN_POINT('',(3.42660065607856,4.87367679877478E-13,4.415875));
#27892=CARTESIAN_POINT('Ctrl Pts',(17.6766006560786,-0.000263771022561289,
4.41536107794487));
#27893=CARTESIAN_POINT('Ctrl Pts',(17.6825487540639,-0.0522183410383149,
4.41566152300153));
#27894=CARTESIAN_POINT('Ctrl Pts',(17.7044021307368,-0.24273028972288,4.38249735042552));
#27895=CARTESIAN_POINT('Ctrl Pts',(17.7421607860973,-0.48225726547346,4.09660825404716));
#27896=CARTESIAN_POINT('Ctrl Pts',(17.7898766221602,-0.342084653792828,
3.64661166616396));
#27897=CARTESIAN_POINT('Ctrl Pts',(17.837592458223,0.112229559114723,3.52113702282083));
#27898=CARTESIAN_POINT('Ctrl Pts',(17.8853082942859,0.463481641013499,3.83540961967535));
#27899=CARTESIAN_POINT('Ctrl Pts',(17.9316443602377,0.391261919872151,4.28736986940801));
#27900=CARTESIAN_POINT('Ctrl Pts',(17.962075147502,0.125831334120538,4.41565069513148));
#27901=CARTESIAN_POINT('Ctrl Pts',(17.9766006560786,-0.000210814279110157,
4.41643020456723));
#27902=CARTESIAN_POINT('Ctrl Pts',(17.7733993439214,-0.000309142357869142,
4.41544738986064));
#27903=CARTESIAN_POINT('Ctrl Pts',(17.7788786337482,-0.0481438769258273,
4.41577602216682));
#27904=CARTESIAN_POINT('Ctrl Pts',(17.8002632022627,-0.23443694547481,4.38601982759396));
#27905=CARTESIAN_POINT('Ctrl Pts',(17.8375530494648,-0.479202773223469,
4.11076970247734));
#27906=CARTESIAN_POINT('Ctrl Pts',(17.8852688855277,-0.352344189444135,
3.65683998336499));
#27907=CARTESIAN_POINT('Ctrl Pts',(17.9329847215905,0.0980774850139738,
3.51803938772416));
#27908=CARTESIAN_POINT('Ctrl Pts',(17.9807005576534,0.458433095867658,3.82183063825345));
#27909=CARTESIAN_POINT('Ctrl Pts',(18.0275054317636,0.3989600628602,4.28031410431705));
#27910=CARTESIAN_POINT('Ctrl Pts',(18.0584050271863,0.129907183855675,4.41591763216682));
#27911=CARTESIAN_POINT('Ctrl Pts',(18.0733993439214,-0.000144384975211439,
4.41650095473263));
#27912=CARTESIAN_POINT('Origin',(3.42660065607856,0.,4.));
#27913=CARTESIAN_POINT('',(17.3766006560786,0.000316824918469052,4.41546566829253));
#27914=CARTESIAN_POINT('',(17.4733993439214,0.000273208168652644,4.41537657040552));
#27915=CARTESIAN_POINT('',(3.42660065607856,4.87367679877478E-13,4.415875));
#27916=CARTESIAN_POINT('Ctrl Pts',(17.3766006560786,0.000316824918469058,
4.41546566829253));
#27917=CARTESIAN_POINT('Ctrl Pts',(17.3871170819382,-0.0914824399419538,
4.4148173972429));
#27918=CARTESIAN_POINT('Ctrl Pts',(17.4135387864855,-0.323087181591141,
4.33950699049548));
#27919=CARTESIAN_POINT('Ctrl Pts',(17.4558657697204,-0.489877595596684,
3.956123284257));
#27920=CARTESIAN_POINT('Ctrl Pts',(17.5035816057832,-0.228040769637767,
3.56422180844494));
#27921=CARTESIAN_POINT('Ctrl Pts',(17.551297441846,0.243209403937772,3.57250215124727));
#27922=CARTESIAN_POINT('Ctrl Pts',(17.5990132779089,0.491116639619549,3.97336034645914));
#27923=CARTESIAN_POINT('Ctrl Pts',(17.6407810159864,0.313340775136121,4.34566293955037));
#27924=CARTESIAN_POINT('Ctrl Pts',(17.6666434753763,0.0867087440962768,
4.41485812965324));
#27925=CARTESIAN_POINT('Ctrl Pts',(17.6766006560786,-0.000263771022561289,
4.41536107794487));
#27926=CARTESIAN_POINT('Ctrl Pts',(17.4733993439214,0.000273208168652693,
4.41537657040552));
#27927=CARTESIAN_POINT('Ctrl Pts',(17.4834469616226,-0.0874810350323011,
4.41484969107387));
#27928=CARTESIAN_POINT('Ctrl Pts',(17.5093998580114,-0.314919534962053,
4.34468516187688));
#27929=CARTESIAN_POINT('Ctrl Pts',(17.5512580330878,-0.490957336521241,
3.97057010757845));
#27930=CARTESIAN_POINT('Ctrl Pts',(17.5989738691507,-0.240776309167652,
3.57112706567612));
#27931=CARTESIAN_POINT('Ctrl Pts',(17.6466897052135,0.230513307714322,3.56552463842171));
#27932=CARTESIAN_POINT('Ctrl Pts',(17.6944055412763,0.490119007219086,3.95890762096741));
#27933=CARTESIAN_POINT('Ctrl Pts',(17.7366420875123,0.321513805022658,4.34052027563639));
#27934=CARTESIAN_POINT('Ctrl Pts',(17.7629733550606,0.090710757213051,4.41482206853766));
#27935=CARTESIAN_POINT('Ctrl Pts',(17.7733993439214,-0.000309142357869142,
4.41544738986064));
#27936=CARTESIAN_POINT('Origin',(3.42660065607856,0.,4.));
#27937=CARTESIAN_POINT('',(17.0766006560786,0.000130763213737631,4.41651185352269));
#27938=CARTESIAN_POINT('',(17.1733993439214,0.000198609043858391,4.41644558073401));
#27939=CARTESIAN_POINT('',(3.42660065607856,4.87367679877478E-13,4.415875));
#27940=CARTESIAN_POINT('Ctrl Pts',(17.0766006560786,0.000130763213737628,
4.41651185352269));
#27941=CARTESIAN_POINT('Ctrl Pts',(17.0916854098125,-0.130696083011285,
4.41597403242798));
#27942=CARTESIAN_POINT('Ctrl Pts',(17.1226754422341,-0.400436570105288,
4.2789290971087));
#27943=CARTESIAN_POINT('Ctrl Pts',(17.1695707533433,-0.457413284126125,
3.81922856321607));
#27944=CARTESIAN_POINT('Ctrl Pts',(17.2172865894061,-0.0953372598908034,
3.51748986360026));
#27945=CARTESIAN_POINT('Ctrl Pts',(17.265002425469,0.354288437054553,3.6588476466131));
#27946=CARTESIAN_POINT('Ctrl Pts',(17.3127182615318,0.478565610824392,4.11349088504481));
#27947=CARTESIAN_POINT('Ctrl Pts',(17.349917671735,0.232837083242772,4.38668157013213));
#27948=CARTESIAN_POINT('Ctrl Pts',(17.3712118032506,0.0473568302064652,
4.41579785693967));
#27949=CARTESIAN_POINT('Ctrl Pts',(17.3766006560786,0.000316824918469058,
4.41546566829253));
#27950=CARTESIAN_POINT('Ctrl Pts',(17.1733993439214,0.000198609043858397,
4.41644558073401));
#27951=CARTESIAN_POINT('Ctrl Pts',(17.1880152894969,-0.126615914365149,
4.41569892234974));
#27952=CARTESIAN_POINT('Ctrl Pts',(17.2185365137601,-0.392752582168809,
4.28602487069057));
#27953=CARTESIAN_POINT('Ctrl Pts',(17.2649630167107,-0.462538907526291,
3.83277863809798));
#27954=CARTESIAN_POINT('Ctrl Pts',(17.3126788527736,-0.109506707187599,
3.52050703244687));
#27955=CARTESIAN_POINT('Ctrl Pts',(17.3603946888365,0.344087187338735,3.64856119684745));
#27956=CARTESIAN_POINT('Ctrl Pts',(17.4081105248993,0.481700523269991,4.09934702176407));
#27957=CARTESIAN_POINT('Ctrl Pts',(17.4457787432609,0.241130489326423,4.3831889686244));
#27958=CARTESIAN_POINT('Ctrl Pts',(17.467541682935,0.0514330574063097,4.41568373580506));
#27959=CARTESIAN_POINT('Ctrl Pts',(17.4733993439214,0.000273208168652693,
4.41537657040552));
#27960=CARTESIAN_POINT('Origin',(3.42660065607856,0.,4.));
#27961=CARTESIAN_POINT('',(16.7766006560786,-0.000383680820852129,4.41586226484778));
#27962=CARTESIAN_POINT('',(16.8733993439214,-0.000374684679869397,4.41598699190495));
#27963=CARTESIAN_POINT('',(3.42660065607856,4.87367679877478E-13,4.415875));
#27964=CARTESIAN_POINT('Ctrl Pts',(16.7766006560786,-0.000383680820852189,
4.41586226484779));
#27965=CARTESIAN_POINT('Ctrl Pts',(16.7803484589992,-0.0330197262611539,
4.41616320579436));
#27966=CARTESIAN_POINT('Ctrl Pts',(16.8000015406075,-0.203823433586872,
4.39772119122577));
#27967=CARTESIAN_POINT('Ctrl Pts',(16.8355599009034,-0.464342533291602,
4.16214572651883));
#27968=CARTESIAN_POINT('Ctrl Pts',(16.8832757369663,-0.387520750342007,
3.69712561530174));
#27969=CARTESIAN_POINT('Ctrl Pts',(16.9309915730291,0.0451673004198413,
3.51023971187451));
#27970=CARTESIAN_POINT('Ctrl Pts',(16.978707409092,0.436377524217892,3.7731082169636));
#27971=CARTESIAN_POINT('Ctrl Pts',(17.0264232451548,0.426855552995382,4.24433493759383));
#27972=CARTESIAN_POINT('Ctrl Pts',(17.0590543274837,0.152277829190936,4.41314658311127));
#27973=CARTESIAN_POINT('Ctrl Pts',(17.0757801311249,0.00724700082869906,
4.41654110793655));
#27974=CARTESIAN_POINT('Ctrl Pts',(17.0766006560786,0.000130763213737628,
4.41651185352269));
#27975=CARTESIAN_POINT('Ctrl Pts',(16.8733993439214,-0.000374684679869387,
4.41598699190495));
#27976=CARTESIAN_POINT('Ctrl Pts',(16.8766783386836,-0.0289064002234668,
4.4162516892709));
#27977=CARTESIAN_POINT('Ctrl Pts',(16.8958626121335,-0.195546116663039,
4.40054826733105));
#27978=CARTESIAN_POINT('Ctrl Pts',(16.9309521642709,-0.459365614209645,
4.17575112327883));
#27979=CARTESIAN_POINT('Ctrl Pts',(16.9786680003337,-0.396272847821079,
3.70867019559999));
#27980=CARTESIAN_POINT('Ctrl Pts',(17.0263838363966,0.0307233721630972,
3.5091219099869));
#27981=CARTESIAN_POINT('Ctrl Pts',(17.0740996724594,0.429505846750062,3.76035452756312));
#27982=CARTESIAN_POINT('Ctrl Pts',(17.1218155085223,0.433866493469502,4.23165726989771));
#27983=CARTESIAN_POINT('Ctrl Pts',(17.1549153990096,0.160507997039396,4.41102293437065));
#27984=CARTESIAN_POINT('Ctrl Pts',(17.1721100108093,0.0113854435377776,
4.41651144656345));
#27985=CARTESIAN_POINT('Ctrl Pts',(17.1733993439214,0.000198609043858397,
4.41644558073401));
#27986=CARTESIAN_POINT('Origin',(3.42660065607856,0.,4.));
#27987=CARTESIAN_POINT('',(16.4766006560786,5.2409936866527E-5,4.41519222098806));
#27988=CARTESIAN_POINT('',(16.5733993439214,-1.52272386678698E-5,4.41518677123726));
#27989=CARTESIAN_POINT('',(3.42660065607856,4.87367679877478E-13,4.415875));
#27990=CARTESIAN_POINT('Ctrl Pts',(16.4766006560786,5.2409936866539E-5,
4.41519222098806));
#27991=CARTESIAN_POINT('Ctrl Pts',(16.4849167868736,-0.0726599781719204,
4.41511070701236));
#27992=CARTESIAN_POINT('Ctrl Pts',(16.5091381963562,-0.284551613766983,
4.36224737480062));
#27993=CARTESIAN_POINT('Ctrl Pts',(16.5492648845264,-0.4912502013546,4.02405128938415));
#27994=CARTESIAN_POINT('Ctrl Pts',(16.5969807205893,-0.285919008936969,
3.59980561575594));
#27995=CARTESIAN_POINT('Ctrl Pts',(16.6446965566521,0.181976008816936,3.54306460296116));
#27996=CARTESIAN_POINT('Ctrl Pts',(16.6924123927149,0.482759657613431,3.90593439612197));
#27997=CARTESIAN_POINT('Ctrl Pts',(16.7363804258571,0.351413532087107,4.31989995948535));
#27998=CARTESIAN_POINT('Ctrl Pts',(16.7644431803116,0.105484194296011,4.41488604428797));
#27999=CARTESIAN_POINT('Ctrl Pts',(16.7766006560786,-0.000383680820852189,
4.41586226484779));
#28000=CARTESIAN_POINT('Ctrl Pts',(16.5733993439214,-1.52272386678906E-5,
4.41518677123726));
#28001=CARTESIAN_POINT('Ctrl Pts',(16.5812466665579,-0.0686308195205231,
4.41520910309265));
#28002=CARTESIAN_POINT('Ctrl Pts',(16.6049992678821,-0.276289552895371,
4.36659242126669));
#28003=CARTESIAN_POINT('Ctrl Pts',(16.6446571478939,-0.490328743065594,
4.03850907134293));
#28004=CARTESIAN_POINT('Ctrl Pts',(16.6923729839567,-0.297581432841348,
3.60840005658827));
#28005=CARTESIAN_POINT('Ctrl Pts',(16.7400888200196,0.168439486040012,3.53790329540825));
#28006=CARTESIAN_POINT('Ctrl Pts',(16.7878046560824,0.479779833116189,3.89175704832657));
#28007=CARTESIAN_POINT('Ctrl Pts',(16.832241497383,0.359412856911567,4.31386464726761));
#28008=CARTESIAN_POINT('Ctrl Pts',(16.860773059996,0.109491163683573,4.41496773315674));
#28009=CARTESIAN_POINT('Ctrl Pts',(16.8733993439214,-0.000374684679869387,
4.41598699190495));
#28010=CARTESIAN_POINT('Origin',(3.42660065607856,0.,4.));
#28011=CARTESIAN_POINT('',(16.1766006560786,0.000364146841390381,4.41605523138122));
#28012=CARTESIAN_POINT('',(16.2733993439214,0.000380345806842055,4.41593091837313));
#28013=CARTESIAN_POINT('',(3.42660065607856,4.87367679877478E-13,4.415875));
#28014=CARTESIAN_POINT('Ctrl Pts',(16.1766006560786,0.000364146841390366,
4.41605523138122));
#28015=CARTESIAN_POINT('Ctrl Pts',(16.1894851147479,-0.111700864104492,
4.41502624848758));
#28016=CARTESIAN_POINT('Ctrl Pts',(16.2182748521048,-0.363797281821349,
4.31045679267864));
#28017=CARTESIAN_POINT('Ctrl Pts',(16.2629698681494,-0.477960913216358,
3.88398883549692));
#28018=CARTESIAN_POINT('Ctrl Pts',(16.3106857042122,-0.160921706883503,
3.53523185446324));
#28019=CARTESIAN_POINT('Ctrl Pts',(16.358401540275,0.303894378979202,3.6132786128531));
#28020=CARTESIAN_POINT('Ctrl Pts',(16.4061173763379,0.489639580609251,4.04645757153336));
#28021=CARTESIAN_POINT('Ctrl Pts',(16.4455170816057,0.271734615807756,4.36891289568356));
#28022=CARTESIAN_POINT('Ctrl Pts',(16.4690115081859,0.0664083969439258,
4.41526660914191));
#28023=CARTESIAN_POINT('Ctrl Pts',(16.4766006560786,5.2409936866539E-5,
4.41519222098806));
#28024=CARTESIAN_POINT('Ctrl Pts',(16.2733993439214,0.000380345806842052,
4.41593091837313));
#28025=CARTESIAN_POINT('Ctrl Pts',(16.2858149944323,-0.107690075887363,
4.41492720978183));
#28026=CARTESIAN_POINT('Ctrl Pts',(16.3141359236307,-0.35582464097624,4.31660057631701));
#28027=CARTESIAN_POINT('Ctrl Pts',(16.3583621315169,-0.481170314810987,
3.89811598262401));
#28028=CARTESIAN_POINT('Ctrl Pts',(16.4060779675797,-0.174540169679895,
3.54017290856226));
#28029=CARTESIAN_POINT('Ctrl Pts',(16.4537938036425,0.292372898913969,3.60449612791703));
#28030=CARTESIAN_POINT('Ctrl Pts',(16.5015096397054,0.490795435699827,4.0320166386149));
#28031=CARTESIAN_POINT('Ctrl Pts',(16.5413781531317,0.280003220364278,4.36466130212541));
#28032=CARTESIAN_POINT('Ctrl Pts',(16.5653413878703,0.0704421061260754,
4.4151638399628));
#28033=CARTESIAN_POINT('Ctrl Pts',(16.5733993439214,-1.52272386678906E-5,
4.41518677123726));
#28034=CARTESIAN_POINT('Origin',(3.42660065607856,0.,4.));
#28035=CARTESIAN_POINT('',(15.8766006560786,-0.00023258108979477,4.41639972388928));
#28036=CARTESIAN_POINT('',(15.9733993439214,-0.000169011902647176,4.4164782780785));
#28037=CARTESIAN_POINT('',(3.42660065607856,4.87367679877478E-13,4.415875));
#28038=CARTESIAN_POINT('Ctrl Pts',(15.8766006560786,-0.000232581089794846,
4.41639972388928));
#28039=CARTESIAN_POINT('Ctrl Pts',(15.8781481639346,-0.0136633580705269,
4.41648966084242));
#28040=CARTESIAN_POINT('Ctrl Pts',(15.8956009504782,-0.165044849757219,
4.40979870506104));
#28041=CARTESIAN_POINT('Ctrl Pts',(15.9289590157095,-0.437567097060412,
4.22458909239344));
#28042=CARTESIAN_POINT('Ctrl Pts',(15.9766748517724,-0.425562075928853,
3.75341909160864));
#28043=CARTESIAN_POINT('Ctrl Pts',(16.0243906878352,-0.0227568523576073,
3.50868813313462));
#28044=CARTESIAN_POINT('Ctrl Pts',(16.072106523898,0.400946338892803,3.71513642180785));
#28045=CARTESIAN_POINT('Ctrl Pts',(16.1198223599609,0.456454337785543,4.1831793175245));
#28046=CARTESIAN_POINT('Ctrl Pts',(16.1546537373544,0.190990792023167,4.40204523666471));
#28047=CARTESIAN_POINT('Ctrl Pts',(16.1735798360603,0.0266382990664043,
4.41629648110721));
#28048=CARTESIAN_POINT('Ctrl Pts',(16.1766006560786,0.000364146841390366,
4.41605523138122));
#28049=CARTESIAN_POINT('Ctrl Pts',(15.9733993439214,-0.000169011902647174,
4.4164782780785));
#28050=CARTESIAN_POINT('Ctrl Pts',(15.974478043619,-0.00952634975615679,
4.4165263696097));
#28051=CARTESIAN_POINT('Ctrl Pts',(15.9914620220042,-0.156808910032117,
4.4119928338179));
#28052=CARTESIAN_POINT('Ctrl Pts',(16.024351279077,-0.430762722000766,4.23737881579128));
#28053=CARTESIAN_POINT('Ctrl Pts',(16.0720671151398,-0.432639725453012,
3.76605963834362));
#28054=CARTESIAN_POINT('Ctrl Pts',(16.1197829512026,-0.0372170120039125,
3.50957149464017));
#28055=CARTESIAN_POINT('Ctrl Pts',(16.1674987872655,0.392382656225717,3.70345139362117));
#28056=CARTESIAN_POINT('Ctrl Pts',(16.2152146233283,0.461651293660056,4.16965644082667));
#28057=CARTESIAN_POINT('Ctrl Pts',(16.2505148088803,0.199264245432362,4.39929555075695));
#28058=CARTESIAN_POINT('Ctrl Pts',(16.2699097157447,0.0307553622657438,
4.41621302761729));
#28059=CARTESIAN_POINT('Ctrl Pts',(16.2733993439214,0.000380345806842052,
4.41593091837313));
#28060=CARTESIAN_POINT('Origin',(3.42660065607856,0.,4.));
#28061=CARTESIAN_POINT('',(15.5766006560786,-0.000245472137683418,4.41533389801214));
#28062=CARTESIAN_POINT('',(15.6733993439214,-0.00029394562308721,4.41541483535501));
#28063=CARTESIAN_POINT('',(3.42660065607856,4.87367679877478E-13,4.415875));
#28064=CARTESIAN_POINT('Ctrl Pts',(15.5766006560786,-0.000245472137683396,
4.41533389801214));
#28065=CARTESIAN_POINT('Ctrl Pts',(15.5827164918089,-0.0536739331835165,
4.41562024719655));
#28066=CARTESIAN_POINT('Ctrl Pts',(15.6047376062269,-0.245697356182912,
4.38119912149661));
#28067=CARTESIAN_POINT('Ctrl Pts',(15.6426639993325,-0.483248643997369,
4.09152034160055));
#28068=CARTESIAN_POINT('Ctrl Pts',(15.6903798353953,-0.338341267922855,
3.64302603558196));
#28069=CARTESIAN_POINT('Ctrl Pts',(15.7380956714582,0.117270100534806,3.52234641383892));
#28070=CARTESIAN_POINT('Ctrl Pts',(15.785811507521,0.465190531238913,3.84030342991275));
#28071=CARTESIAN_POINT('Ctrl Pts',(15.8319798357278,0.388490242362186,4.28984418805176));
#28072=CARTESIAN_POINT('Ctrl Pts',(15.862242885247,0.124378106492246,4.41556528924811));
#28073=CARTESIAN_POINT('Ctrl Pts',(15.8766006560786,-0.000232581089794846,
4.41639972388928));
#28074=CARTESIAN_POINT('Ctrl Pts',(15.6733993439214,-0.000293945623087231,
4.41541483535501));
#28075=CARTESIAN_POINT('Ctrl Pts',(15.6790463714933,-0.0496027558454661,
4.41573527017753));
#28076=CARTESIAN_POINT('Ctrl Pts',(15.7005986777528,-0.23740431922453,4.38477730872224));
#28077=CARTESIAN_POINT('Ctrl Pts',(15.7380562626999,-0.480343569999647,
4.1057131950703));
#28078=CARTESIAN_POINT('Ctrl Pts',(15.7857720987628,-0.348708030819167,
3.6531456586776));
#28079=CARTESIAN_POINT('Ctrl Pts',(15.8334879348256,0.103151458625294,3.5190998009613));
#28080=CARTESIAN_POINT('Ctrl Pts',(15.8812037708885,0.460285376424935,3.82667199562295));
#28081=CARTESIAN_POINT('Ctrl Pts',(15.9278409072537,0.396214095655672,4.28286244744368));
#28082=CARTESIAN_POINT('Ctrl Pts',(15.9585727649314,0.128446309981357,4.41581726659612));
#28083=CARTESIAN_POINT('Ctrl Pts',(15.9733993439214,-0.000169011902647174,
4.4164782780785));
#28084=CARTESIAN_POINT('Origin',(3.42660065607856,0.,4.));
#28085=CARTESIAN_POINT('',(15.2766006560786,0.000330084823988869,4.41550084660604));
#28086=CARTESIAN_POINT('',(15.3733993439214,0.000289868078815952,4.41540680128743));
#28087=CARTESIAN_POINT('',(3.42660065607856,4.87367679877478E-13,4.415875));
#28088=CARTESIAN_POINT('Ctrl Pts',(15.2766006560786,0.000330084823988861,
4.41550084660604));
#28089=CARTESIAN_POINT('Ctrl Pts',(15.2872848196833,-0.0929135079625664,
4.41481081573461));
#28090=CARTESIAN_POINT('Ctrl Pts',(15.3138742619755,-0.32600240339937,4.33760928826424));
#28091=CARTESIAN_POINT('Ctrl Pts',(15.3563689829555,-0.489387968817152,
3.95096286275689));
#28092=CARTESIAN_POINT('Ctrl Pts',(15.4040848190183,-0.223435404337718,
3.56184267101825));
#28093=CARTESIAN_POINT('Ctrl Pts',(15.4518006550811,0.24770132994065,3.57508909640066));
#28094=CARTESIAN_POINT('Ctrl Pts',(15.499516491144,0.491370121559653,3.97853774265298));
#28095=CARTESIAN_POINT('Ctrl Pts',(15.5411164914764,0.310410063586636,4.3474585185963));
#28096=CARTESIAN_POINT('Ctrl Pts',(15.5668112131213,0.0852759340546689,
4.41487554708019));
#28097=CARTESIAN_POINT('Ctrl Pts',(15.5766006560786,-0.000245472137683396,
4.41533389801214));
#28098=CARTESIAN_POINT('Ctrl Pts',(15.3733993439214,0.000289868078815973,
4.41540680128743));
#28099=CARTESIAN_POINT('Ctrl Pts',(15.3836146993676,-0.0889130762729256,
4.41483587894927));
#28100=CARTESIAN_POINT('Ctrl Pts',(15.4097353335015,-0.317845114095608,
4.34285359523591));
#28101=CARTESIAN_POINT('Ctrl Pts',(15.4517612463229,-0.490619905976795,
3.96539750426199));
#28102=CARTESIAN_POINT('Ctrl Pts',(15.4994770823858,-0.236243011612202,
3.56861332390027));
#28103=CARTESIAN_POINT('Ctrl Pts',(15.5471929184486,0.235079475381852,3.56797816593814));
#28104=CARTESIAN_POINT('Ctrl Pts',(15.5949087545115,0.490524862970081,3.9640753057054));
#28105=CARTESIAN_POINT('Ctrl Pts',(15.6369775630024,0.318592711010818,4.34238143198936));
#28106=CARTESIAN_POINT('Ctrl Pts',(15.6631410928057,0.0892792238074376,
4.41483274135358));
#28107=CARTESIAN_POINT('Ctrl Pts',(15.6733993439214,-0.000293945623087231,
4.41541483535501));
#28108=CARTESIAN_POINT('Origin',(3.42660065607856,0.,4.));
#28109=CARTESIAN_POINT('',(14.9766006560786,0.000104941934236194,4.41652945172571));
#28110=CARTESIAN_POINT('',(15.0733993439214,0.000175165248676303,4.41647198785975));
#28111=CARTESIAN_POINT('',(3.42660065607856,4.87367679877478E-13,4.415875));
#28112=CARTESIAN_POINT('Ctrl Pts',(14.9766006560786,0.000104941934236227,
4.41652945172572));
#28113=CARTESIAN_POINT('Ctrl Pts',(14.9918531475576,-0.132161740438444,
4.41608294134065));
#28114=CARTESIAN_POINT('Ctrl Pts',(15.0230109177242,-0.40316752945992,4.27633971254324));
#28115=CARTESIAN_POINT('Ctrl Pts',(15.0700739665785,-0.455482716161518,
3.8144178884426));
#28116=CARTESIAN_POINT('Ctrl Pts',(15.1177898026413,-0.0902467530057116,
3.51651189422706));
#28117=CARTESIAN_POINT('Ctrl Pts',(15.1655056387041,0.357864192060027,3.66260046696357));
#28118=CARTESIAN_POINT('Ctrl Pts',(15.2132214747669,0.47734294310866,4.11852822244656));
#28119=CARTESIAN_POINT('Ctrl Pts',(15.2502531472251,0.229869832763757,4.3878938710325));
#28120=CARTESIAN_POINT('Ctrl Pts',(15.2713795409956,0.0458961718568525,
4.41583804947224));
#28121=CARTESIAN_POINT('Ctrl Pts',(15.2766006560786,0.000330084823988861,
4.41550084660604));
#28122=CARTESIAN_POINT('Ctrl Pts',(15.0733993439214,0.000175165248676341,
4.41647198785975));
#28123=CARTESIAN_POINT('Ctrl Pts',(15.0881830272419,-0.128073190246274,
4.41579247653651));
#28124=CARTESIAN_POINT('Ctrl Pts',(15.1188719892501,-0.395510344386944,
4.28350986851547));
#28125=CARTESIAN_POINT('Ctrl Pts',(15.1654662299459,-0.46075086019608,3.82791319143947));
#28126=CARTESIAN_POINT('Ctrl Pts',(15.2131820660087,-0.104447211543591,
3.51937956259357));
#28127=CARTESIAN_POINT('Ctrl Pts',(15.2608979020716,0.347771918596306,3.652207076714));
#28128=CARTESIAN_POINT('Ctrl Pts',(15.3086137381344,0.480626744730421,4.10441818376995));
#28129=CARTESIAN_POINT('Ctrl Pts',(15.346114218751,0.238163166260598,4.38445638366753));
#28130=CARTESIAN_POINT('Ctrl Pts',(15.36770942068,0.0499756483669043,4.41572480336754));
#28131=CARTESIAN_POINT('Ctrl Pts',(15.3733993439214,0.000289868078815973,
4.41540680128743));
#28132=CARTESIAN_POINT('Origin',(3.42660065607856,0.,4.));
#28133=CARTESIAN_POINT('',(14.6766006560786,-0.000383732061438463,4.41581798673635));
#28134=CARTESIAN_POINT('',(14.7733993439214,-0.000379407362125217,4.41594234696178));
#28135=CARTESIAN_POINT('',(3.42660065607856,4.87367679877478E-13,4.415875));
#28136=CARTESIAN_POINT('Ctrl Pts',(14.6766006560786,-0.000383732061438387,
4.41581798673635));
#28137=CARTESIAN_POINT('Ctrl Pts',(14.6805161967443,-0.0344897130604965,
4.41612948839573));
#28138=CARTESIAN_POINT('Ctrl Pts',(14.7003370160976,-0.206786574235377,
4.39667515056147));
#28139=CARTESIAN_POINT('Ctrl Pts',(14.7360631141386,-0.466025611307368,
4.15724297904063));
#28140=CARTESIAN_POINT('Ctrl Pts',(14.7837789502014,-0.38430721152129,3.69305832471834));
#28141=CARTESIAN_POINT('Ctrl Pts',(14.8314947862642,0.0503264139313189,
3.51074293371195));
#28142=CARTESIAN_POINT('Ctrl Pts',(14.8792106223271,0.438744519099385,3.77771983486548));
#28143=CARTESIAN_POINT('Ctrl Pts',(14.9269264583899,0.42425678142631,4.24882003188202));
#28144=CARTESIAN_POINT('Ctrl Pts',(14.9593898029737,0.149335702075518,4.41387566524124));
#28145=CARTESIAN_POINT('Ctrl Pts',(14.97594786887,0.00576578747519492,4.41654856180149));
#28146=CARTESIAN_POINT('Ctrl Pts',(14.9766006560786,0.000104941934236227,
4.41652945172572));
#28147=CARTESIAN_POINT('Ctrl Pts',(14.7733993439214,-0.000379407362125234,
4.41594234696178));
#28148=CARTESIAN_POINT('Ctrl Pts',(14.7768460764287,-0.0303789312965351,
4.41622104989506));
#28149=CARTESIAN_POINT('Ctrl Pts',(14.7961980876235,-0.198506931257387,
4.39955296987463));
#28150=CARTESIAN_POINT('Ctrl Pts',(14.831455377506,-0.461192356972643,4.17090007232882));
#28151=CARTESIAN_POINT('Ctrl Pts',(14.8791712135689,-0.393180492164677,
3.7045100248179));
#28152=CARTESIAN_POINT('Ctrl Pts',(14.9268870496317,0.0358950684576197,
3.50947296821438));
#28153=CARTESIAN_POINT('Ctrl Pts',(14.9746028856945,0.432007635398663,3.76489443262817));
#28154=CARTESIAN_POINT('Ctrl Pts',(15.0223187217574,0.431400943461215,4.23621695712364));
#28155=CARTESIAN_POINT('Ctrl Pts',(15.0552508744997,0.157562060208247,4.41179740605063));
#28156=CARTESIAN_POINT('Ctrl Pts',(15.0722777485543,0.00990499767517082,
4.41652354042182));
#28157=CARTESIAN_POINT('Ctrl Pts',(15.0733993439214,0.000175165248676341,
4.41647198785975));
#28158=CARTESIAN_POINT('Origin',(3.42660065607856,0.,4.));
#28159=CARTESIAN_POINT('',(14.3766006560786,7.63317591858645E-5,4.41519896243726));
#28160=CARTESIAN_POINT('',(14.4733993439214,9.02664646690309E-6,4.41518644689786));
#28161=CARTESIAN_POINT('',(3.42660065607856,4.87367679877478E-13,4.415875));
#28162=CARTESIAN_POINT('Ctrl Pts',(14.3766006560786,7.63317591858798E-5,
4.41519896243726));
#28163=CARTESIAN_POINT('Ctrl Pts',(14.3850845246186,-0.0740996743586071,
4.41507773880187));
#28164=CARTESIAN_POINT('Ctrl Pts',(14.4094736718463,-0.287504468978829,
4.360651101065));
#28165=CARTESIAN_POINT('Ctrl Pts',(14.4497680977616,-0.491476396904638,
4.01887262932433));
#28166=CARTESIAN_POINT('Ctrl Pts',(14.4974839338244,-0.281685449746218,
3.59681451879656));
#28167=CARTESIAN_POINT('Ctrl Pts',(14.5451997698872,0.186781580201919,3.54500783946397));
#28168=CARTESIAN_POINT('Ctrl Pts',(14.59291560595,0.483724211046603,3.91102746210588));
#28169=CARTESIAN_POINT('Ctrl Pts',(14.6367159013472,0.348540265561382,4.32201186060262));
#28170=CARTESIAN_POINT('Ctrl Pts',(14.6646109180567,0.104051852208848,4.41486414061182));
#28171=CARTESIAN_POINT('Ctrl Pts',(14.6766006560786,-0.000383732061438387,
4.41581798673635));
#28172=CARTESIAN_POINT('Ctrl Pts',(14.4733993439214,9.0266464668684E-6,
4.41518644689786));
#28173=CARTESIAN_POINT('Ctrl Pts',(14.481414404303,-0.0700733710850898,
4.41517292627706));
#28174=CARTESIAN_POINT('Ctrl Pts',(14.5053347433722,-0.279247125311621,
4.3650573561381));
#28175=CARTESIAN_POINT('Ctrl Pts',(14.545160361129,-0.490707361486496,4.03333931965322));
#28176=CARTESIAN_POINT('Ctrl Pts',(14.5928761971918,-0.293437803431633,
3.60528557111603));
#28177=CARTESIAN_POINT('Ctrl Pts',(14.6405920332547,0.173300204635467,3.53970415608515));
#28178=CARTESIAN_POINT('Ctrl Pts',(14.6883078693175,0.480893968219416,3.89681949708321));
#28179=CARTESIAN_POINT('Ctrl Pts',(14.7325769728731,0.356556173733762,4.31604662460621));
#28180=CARTESIAN_POINT('Ctrl Pts',(14.760940797741,0.10805675748006,4.41493494840171));
#28181=CARTESIAN_POINT('Ctrl Pts',(14.7733993439214,-0.000379407362125234,
4.41594234696178));
#28182=CARTESIAN_POINT('Origin',(3.42660065607856,0.,4.));
#28183=CARTESIAN_POINT('',(14.0766006560786,0.000355193352615291,4.41609897421413));
#28184=CARTESIAN_POINT('',(14.1733993439214,0.000376051973931104,4.41597558743442));
#28185=CARTESIAN_POINT('',(3.42660065607856,4.87367679877478E-13,4.415875));
#28186=CARTESIAN_POINT('Ctrl Pts',(14.0766006560786,0.000355193352615277,
4.41609897421413));
#28187=CARTESIAN_POINT('Ctrl Pts',(14.0896528524929,-0.113137957382804,
4.41506966208575));
#28188=CARTESIAN_POINT('Ctrl Pts',(14.1186103275949,-0.366637448157006,
4.30821039815648));
#28189=CARTESIAN_POINT('Ctrl Pts',(14.1634730813845,-0.476711717661702,
3.87895801102093));
#28190=CARTESIAN_POINT('Ctrl Pts',(14.2111889174473,-0.156014541823709,
3.53356170012368));
#28191=CARTESIAN_POINT('Ctrl Pts',(14.2589047535102,0.307953188363286,3.61650285707861));
#28192=CARTESIAN_POINT('Ctrl Pts',(14.306620589573,0.4891227672074,4.05161534124029));
#28193=CARTESIAN_POINT('Ctrl Pts',(14.3458525570958,0.268773633406098,4.37039329245586));
#28194=CARTESIAN_POINT('Ctrl Pts',(14.369179245931,0.0649630708582953,4.4153050049005));
#28195=CARTESIAN_POINT('Ctrl Pts',(14.3766006560786,7.63317591858798E-5,
4.41519896243726));
#28196=CARTESIAN_POINT('Ctrl Pts',(14.1733993439214,0.000376051973931098,
4.41597558743442));
#28197=CARTESIAN_POINT('Ctrl Pts',(14.1859827321773,-0.109124255432428,
4.41495896305428));
#28198=CARTESIAN_POINT('Ctrl Pts',(14.2144713991208,-0.358682910161539,
4.31442504752535));
#28199=CARTESIAN_POINT('Ctrl Pts',(14.258865344752,-0.480069828122688,3.8930505494253));
#28200=CARTESIAN_POINT('Ctrl Pts',(14.3065811808148,-0.169684322438749,
3.53835895376334));
#28201=CARTESIAN_POINT('Ctrl Pts',(14.3542970168777,0.296524907469595,3.60759943412104));
#28202=CARTESIAN_POINT('Ctrl Pts',(14.4020128529405,0.49043075222644,4.0371873919842));
#28203=CARTESIAN_POINT('Ctrl Pts',(14.4417136286217,0.277046036654804,4.36620192284859));
#28204=CARTESIAN_POINT('Ctrl Pts',(14.4655091256154,0.0689998253659925,
4.41519975692232));
#28205=CARTESIAN_POINT('Ctrl Pts',(14.4733993439214,9.0266464668684E-6,
4.41518644689786));
#28206=CARTESIAN_POINT('Origin',(3.42660065607856,0.,4.));
#28207=CARTESIAN_POINT('',(13.7766006560786,-0.000253139125078747,4.41636688691614));
#28208=CARTESIAN_POINT('',(13.8733993439214,-0.000192710833643805,4.4164526008213));
#28209=CARTESIAN_POINT('',(3.42660065607856,4.87367679877478E-13,4.415875));
#28210=CARTESIAN_POINT('Ctrl Pts',(13.7766006560786,-0.000253139125078718,
4.41636688691614));
#28211=CARTESIAN_POINT('Ctrl Pts',(13.7783159016796,-0.0151427949580853,
4.41647347977994));
#28212=CARTESIAN_POINT('Ctrl Pts',(13.7959364259683,-0.167994124135391,
4.40898222403799));
#28213=CARTESIAN_POINT('Ctrl Pts',(13.8294622289446,-0.439909757638992,
4.21996506537626));
#28214=CARTESIAN_POINT('Ctrl Pts',(13.8771780650075,-0.422939705734467,
3.74894775411238));
#28215=CARTESIAN_POINT('Ctrl Pts',(13.9248939010703,-0.0175776142901187,
3.50847558318244));
#28216=CARTESIAN_POINT('Ctrl Pts',(13.9726097371332,0.403926270823208,3.71937784729135));
#28217=CARTESIAN_POINT('Ctrl Pts',(14.020325573196,0.454498446235019,4.18797975215946));
#28218=CARTESIAN_POINT('Ctrl Pts',(14.0549892128445,0.188032430710383,4.40299531219535));
#28219=CARTESIAN_POINT('Ctrl Pts',(14.0737475738053,0.0251636842930195,
4.41632397176197));
#28220=CARTESIAN_POINT('Ctrl Pts',(14.0766006560786,0.000355193352615277,
4.41609897421413));
#28221=CARTESIAN_POINT('Ctrl Pts',(13.8733993439214,-0.000192710833643682,
4.4164526008213));
#28222=CARTESIAN_POINT('Ctrl Pts',(13.874645781364,-0.0110068809386406,
4.41651469495978));
#28223=CARTESIAN_POINT('Ctrl Pts',(13.8917974974943,-0.15975450351916,4.41122255187585));
#28224=CARTESIAN_POINT('Ctrl Pts',(13.9248544923121,-0.433240552373761,
4.23282579030437));
#28225=CARTESIAN_POINT('Ctrl Pts',(13.9725703283749,-0.430150181893835,
3.76151300691929));
#28226=CARTESIAN_POINT('Ctrl Pts',(14.0202861644378,-0.032046280669499,
3.50920649887429));
#28227=CARTESIAN_POINT('Ctrl Pts',(14.0680020005006,0.39548621318905,3.70760321474174));
#28228=CARTESIAN_POINT('Ctrl Pts',(14.1157178365634,0.459837632138507,4.1745123976147));
#28229=CARTESIAN_POINT('Ctrl Pts',(14.1508502843704,0.196303200904851,4.40029544879449));
#28230=CARTESIAN_POINT('Ctrl Pts',(14.1700774534897,0.0292830534939708,
4.41624396624722));
#28231=CARTESIAN_POINT('Ctrl Pts',(14.1733993439214,0.000376051973931098,
4.41597558743442));
#28232=CARTESIAN_POINT('Origin',(3.42660065607856,0.,4.));
#28233=CARTESIAN_POINT('',(13.4766006560786,-0.000226204729293368,4.4153088088013));
#28234=CARTESIAN_POINT('',(13.5733993439214,-0.000277574767750837,4.41538411867388));
#28235=CARTESIAN_POINT('',(3.42660065607856,4.87367679877478E-13,4.415875));
#28236=CARTESIAN_POINT('Ctrl Pts',(13.4766006560786,-0.000226204729293314,
4.4153088088013));
#28237=CARTESIAN_POINT('Ctrl Pts',(13.482884229554,-0.0551283395969922,
4.41557894444213));
#28238=CARTESIAN_POINT('Ctrl Pts',(13.505073081717,-0.248664136397309,4.37988069596112));
#28239=CARTESIAN_POINT('Ctrl Pts',(13.5431672125676,-0.484186345555107,
4.08642226350871));
#28240=CARTESIAN_POINT('Ctrl Pts',(13.5908830486304,-0.334560300710407,
3.63948005597396));
#28241=CARTESIAN_POINT('Ctrl Pts',(13.6385988846933,0.122297616148583,3.52360886035071));
#28242=CARTESIAN_POINT('Ctrl Pts',(13.6863147207561,0.466847750307624,3.8452149784873));
#28243=CARTESIAN_POINT('Ctrl Pts',(13.7323153112179,0.38570983934117,4.29229218593957));
#28244=CARTESIAN_POINT('Ctrl Pts',(13.762410622992,0.122927301498021,4.41548505619568));
#28245=CARTESIAN_POINT('Ctrl Pts',(13.7766006560786,-0.000253139125078718,
4.41636688691614));
#28246=CARTESIAN_POINT('Ctrl Pts',(13.5733993439214,-0.000277574767750817,
4.41538411867388));
#28247=CARTESIAN_POINT('Ctrl Pts',(13.5792141092383,-0.0510604653080308,
4.41569425641003));
#28248=CARTESIAN_POINT('Ctrl Pts',(13.6009341532429,-0.240371663949131,
4.38351498152559));
#28249=CARTESIAN_POINT('Ctrl Pts',(13.6385594759351,-0.481431012491488,
4.10064494554323));
#28250=CARTESIAN_POINT('Ctrl Pts',(13.6862753119979,-0.345033139360895,
3.64948986092447));
#28251=CARTESIAN_POINT('Ctrl Pts',(13.7339911480608,0.108213974662067,3.52021363031051));
#28252=CARTESIAN_POINT('Ctrl Pts',(13.7817069841236,0.462086530666827,3.83153260544464));
#28253=CARTESIAN_POINT('Ctrl Pts',(13.8281763827438,0.393458703070077,4.28538422885222));
#28254=CARTESIAN_POINT('Ctrl Pts',(13.8587405026764,0.126988323162951,4.4157223370415));
#28255=CARTESIAN_POINT('Ctrl Pts',(13.8733993439214,-0.000192710833643682,
4.4164526008213));
#28256=CARTESIAN_POINT('Origin',(3.42660065607856,0.,4.));
#28257=CARTESIAN_POINT('',(13.1766006560786,0.000342007958933446,4.41553758638116));
#28258=CARTESIAN_POINT('',(13.2733993439214,0.000305371599794934,4.41543889539504));
#28259=CARTESIAN_POINT('',(3.42660065607856,4.87367679877478E-13,4.415875));
#28260=CARTESIAN_POINT('Ctrl Pts',(13.1766006560786,0.000342007958933428,
4.41553758638117));
#28261=CARTESIAN_POINT('Ctrl Pts',(13.1874525574283,-0.0943443719380771,
4.41480703635833));
#28262=CARTESIAN_POINT('Ctrl Pts',(13.2142097374657,-0.328913583769224,
4.33568767983454));
#28263=CARTESIAN_POINT('Ctrl Pts',(13.2568721961906,-0.488843983144383,
3.94580788806928));
#28264=CARTESIAN_POINT('Ctrl Pts',(13.3045880322534,-0.218805220893238,
3.55951220202843));
#28265=CARTESIAN_POINT('Ctrl Pts',(13.3523038683163,0.252165742455243,3.57772323864086));
#28266=CARTESIAN_POINT('Ctrl Pts',(13.4000197043791,0.491569024438394,3.98371752277252));
#28267=CARTESIAN_POINT('Ctrl Pts',(13.4414519669665,0.307476227900318,4.34923088347422));
#28268=CARTESIAN_POINT('Ctrl Pts',(13.4669789508664,0.0838425436168888,
4.41489516431802));
#28269=CARTESIAN_POINT('Ctrl Pts',(13.4766006560786,-0.000226204729293314,
4.4153088088013));
#28270=CARTESIAN_POINT('Ctrl Pts',(13.2733993439214,0.000305371599794949,
4.41543889539504));
#28271=CARTESIAN_POINT('Ctrl Pts',(13.2837824371127,-0.0903447040275099,
4.41482455235666));
#28272=CARTESIAN_POINT('Ctrl Pts',(13.3100708089916,-0.320767143545349,
4.3409984814332));
#28273=CARTESIAN_POINT('Ctrl Pts',(13.352264459558,-0.490227979701372,3.96022874442655));
#28274=CARTESIAN_POINT('Ctrl Pts',(13.3999802956209,-0.23168347330409,3.56614749850931));
#28275=CARTESIAN_POINT('Ctrl Pts',(13.4476961316837,0.239619531536799,3.57047968038978));
#28276=CARTESIAN_POINT('Ctrl Pts',(13.4954119677466,0.490876233547033,3.96924698078795));
#28277=CARTESIAN_POINT('Ctrl Pts',(13.5373130384925,0.315668023336251,4.34421900798688));
#28278=CARTESIAN_POINT('Ctrl Pts',(13.5633088305507,0.0878472949503496,
4.41484592860038));
#28279=CARTESIAN_POINT('Ctrl Pts',(13.5733993439214,-0.000277574767750817,
4.41538411867388));
#28280=CARTESIAN_POINT('Origin',(3.42660065607856,0.,4.));
#28281=CARTESIAN_POINT('',(12.8766006560786,7.85109994957766E-5,4.41654344863055));
#28282=CARTESIAN_POINT('',(12.9733993439214,0.000150764780949702,4.41649545414489));
#28283=CARTESIAN_POINT('',(3.42660065607856,4.87367679877478E-13,4.415875));
#28284=CARTESIAN_POINT('Ctrl Pts',(12.8766006560786,7.85109994958138E-5,
4.41654344863055));
#28285=CARTESIAN_POINT('Ctrl Pts',(12.8920208853026,-0.133630732206743,
4.41619751255639));
#28286=CARTESIAN_POINT('Ctrl Pts',(12.9233463932143,-0.405888408666218,
4.27372356364211));
#28287=CARTESIAN_POINT('Ctrl Pts',(12.9705771798136,-0.453501555338242,
3.80962782724943));
#28288=CARTESIAN_POINT('Ctrl Pts',(13.0182930158764,-0.0851462219395619,
3.51558762841831));
#28289=CARTESIAN_POINT('Ctrl Pts',(13.0660088519392,0.361400197209248,3.66639076405307));
#28290=CARTESIAN_POINT('Ctrl Pts',(13.1137246880021,0.476067254403989,4.1235523942958));
#28291=CARTESIAN_POINT('Ctrl Pts',(13.1505886227152,0.226902767145371,4.38908671404106));
#28292=CARTESIAN_POINT('Ctrl Pts',(13.1715472787407,0.0444343739838573,
4.41587777975472));
#28293=CARTESIAN_POINT('Ctrl Pts',(13.1766006560786,0.000342007958933428,
4.41553758638117));
#28294=CARTESIAN_POINT('Ctrl Pts',(12.9733993439214,0.000150764780949724,
4.4164954541449));
#28295=CARTESIAN_POINT('Ctrl Pts',(12.988350764987,-0.12953330947047,4.41589144324702));
#28296=CARTESIAN_POINT('Ctrl Pts',(13.0192074647402,-0.39825874617628,4.28096832590395));
#28297=CARTESIAN_POINT('Ctrl Pts',(13.065969443181,-0.458911634846768,3.82306685936703));
#28298=CARTESIAN_POINT('Ctrl Pts',(13.1136852792439,-0.0993761143989603,
3.51830547777773));
#28299=CARTESIAN_POINT('Ctrl Pts',(13.1614011153067,0.351418020999476,3.65589158776806));
#28300=CARTESIAN_POINT('Ctrl Pts',(13.2091169513695,0.479499580452807,4.10947774749948));
#28301=CARTESIAN_POINT('Ctrl Pts',(13.2464496942411,0.235195791588524,4.38570395495548));
#28302=CARTESIAN_POINT('Ctrl Pts',(13.2678771584251,0.0485170676377186,
4.41576563003508));
#28303=CARTESIAN_POINT('Ctrl Pts',(13.2733993439214,0.000305371599794949,
4.41543889539504));
#28304=CARTESIAN_POINT('Origin',(3.42660065607856,0.,4.));
#28305=CARTESIAN_POINT('',(12.5766006560786,-0.000382134531266273,4.41577416496379));
#28306=CARTESIAN_POINT('',(12.6733993439214,-0.000382453243898073,4.41589767499446));
#28307=CARTESIAN_POINT('',(3.42660065607856,4.87367679877478E-13,4.415875));
#28308=CARTESIAN_POINT('Ctrl Pts',(12.5766006560786,-0.000382134531266193,
4.41577416496379));
#28309=CARTESIAN_POINT('Ctrl Pts',(12.5806839344893,-0.0359587315295452,
4.41609477791077));
#28310=CARTESIAN_POINT('Ctrl Pts',(12.6006724915877,-0.209750441210566,
4.39561070447123));
#28311=CARTESIAN_POINT('Ctrl Pts',(12.6365663273737,-0.4676569254097,4.15232276575852));
#28312=CARTESIAN_POINT('Ctrl Pts',(12.6842821634365,-0.381050985679211,
3.68902512775968));
#28313=CARTESIAN_POINT('Ctrl Pts',(12.7319979994994,0.0554799374235607,
3.5113004999026));
#28314=CARTESIAN_POINT('Ctrl Pts',(12.7797138355622,0.441062780321708,3.78235614259331));
#28315=CARTESIAN_POINT('Ctrl Pts',(12.8274296716251,0.421610885427219,4.2532774884218));
#28316=CARTESIAN_POINT('Ctrl Pts',(12.8597252784638,0.146394963767536,4.4145887178469));
#28317=CARTESIAN_POINT('Ctrl Pts',(12.876115606615,0.00428438860018927,
4.4165543301878));
#28318=CARTESIAN_POINT('Ctrl Pts',(12.8766006560786,7.85109994958138E-5,
4.41654344863055));
#28319=CARTESIAN_POINT('Ctrl Pts',(12.6733993439214,-0.000382453243898042,
4.41589767499447));
#28320=CARTESIAN_POINT('Ctrl Pts',(12.6770138141737,-0.0318505807336982,
4.4161892599907));
#28321=CARTESIAN_POINT('Ctrl Pts',(12.6965335631136,-0.201468625965512,
4.39853963407534));
#28322=CARTESIAN_POINT('Ctrl Pts',(12.7319585907412,-0.462967872677167,
4.16603003860975));
#28323=CARTESIAN_POINT('Ctrl Pts',(12.779674426804,-0.390044463885,3.70038267566003));
#28324=CARTESIAN_POINT('Ctrl Pts',(12.8273902628668,0.0410627776982723,
3.50987851185683));
#28325=CARTESIAN_POINT('Ctrl Pts',(12.8751060989297,0.434461438689172,3.76946045210395));
#28326=CARTESIAN_POINT('Ctrl Pts',(12.9228219349925,0.42888747548329,4.24075040649094));
#28327=CARTESIAN_POINT('Ctrl Pts',(12.9555863499897,0.154617472482897,4.41255553662561));
#28328=CARTESIAN_POINT('Ctrl Pts',(12.9724454862994,0.00842423538524961,
4.41653398830136));
#28329=CARTESIAN_POINT('Ctrl Pts',(12.9733993439214,0.000150764780949724,
4.4164954541449));
#28330=CARTESIAN_POINT('Origin',(3.42660065607856,0.,4.));
#28331=CARTESIAN_POINT('',(12.2766006560786,9.99581421417901E-5,4.41520820259509));
#28332=CARTESIAN_POINT('',(12.3733993439214,3.32456539758885E-5,4.41518865831861));
#28333=CARTESIAN_POINT('',(3.42660065607856,4.87367679877478E-13,4.415875));
#28334=CARTESIAN_POINT('Ctrl Pts',(12.2766006560786,9.99581421418094E-5,
4.41520820259509));
#28335=CARTESIAN_POINT('Ctrl Pts',(12.2852522623637,-0.0755384113923865,
4.41504611816934));
#28336=CARTESIAN_POINT('Ctrl Pts',(12.3098091473364,-0.290455378639464,
4.35903266527152));
#28337=CARTESIAN_POINT('Ctrl Pts',(12.3502713109967,-0.49164800158875,4.0136918729824));
#28338=CARTESIAN_POINT('Ctrl Pts',(12.3979871470595,-0.277420602272412,
3.59386820576715));
#28339=CARTESIAN_POINT('Ctrl Pts',(12.4457029831224,0.191566404775332,3.54700161433684));
#28340=CARTESIAN_POINT('Ctrl Pts',(12.4934188191852,0.484635034689867,3.91613041073711));
#28341=CARTESIAN_POINT('Ctrl Pts',(12.5370513768373,0.345661459897227,4.32409890635003));
#28342=CARTESIAN_POINT('Ctrl Pts',(12.5647786558017,0.102620036091023,4.41484591908716));
#28343=CARTESIAN_POINT('Ctrl Pts',(12.5766006560786,-0.000382134531266193,
4.41577416496379));
#28344=CARTESIAN_POINT('Ctrl Pts',(12.3733993439214,3.32456539758746E-5,
4.41518865831861));
#28345=CARTESIAN_POINT('Ctrl Pts',(12.381582142048,-0.071514873974996,4.41513780400291));
#28346=CARTESIAN_POINT('Ctrl Pts',(12.4056702188623,-0.282203129244181,
4.36350051499509));
#28347=CARTESIAN_POINT('Ctrl Pts',(12.4456635743641,-0.491031474462283,
4.0281658647901));
#28348=CARTESIAN_POINT('Ctrl Pts',(12.493379410427,-0.289261580343189,3.60221492864948));
#28349=CARTESIAN_POINT('Ctrl Pts',(12.5410952464898,0.178141673866572,3.54155614424011));
#28350=CARTESIAN_POINT('Ctrl Pts',(12.5888110825527,0.481954687902679,3.90189340664049));
#28351=CARTESIAN_POINT('Ctrl Pts',(12.6329124483632,0.353693368040787,4.31820342736526));
#28352=CARTESIAN_POINT('Ctrl Pts',(12.6611085354861,0.106623193447456,4.41490615616012));
#28353=CARTESIAN_POINT('Ctrl Pts',(12.6733993439214,-0.000382453243898042,
4.41589767499447));
#28354=CARTESIAN_POINT('Origin',(3.42660065607856,0.,4.));
#28355=CARTESIAN_POINT('',(11.9766006560786,0.000344603143201134,4.41614202049347));
#28356=CARTESIAN_POINT('',(12.0733993439214,0.00037008249145147,4.41602009379307));
#28357=CARTESIAN_POINT('',(3.42660065607856,4.87367679877478E-13,4.415875));
#28358=CARTESIAN_POINT('Ctrl Pts',(11.9766006560786,0.000344603143201134,
4.41614202049347));
#28359=CARTESIAN_POINT('Ctrl Pts',(11.989820590238,-0.114576335025177,4.41511745277426));
#28360=CARTESIAN_POINT('Ctrl Pts',(12.018945803085,-0.369470719226983,4.30593844396252));
#28361=CARTESIAN_POINT('Ctrl Pts',(12.0639762946196,-0.475409571231627,
3.87394063131468));
#28362=CARTESIAN_POINT('Ctrl Pts',(12.1116921306825,-0.151090047408964,
3.53194335553704));
#28363=CARTESIAN_POINT('Ctrl Pts',(12.1594079667453,0.311977791768556,3.61976969834691));
#28364=CARTESIAN_POINT('Ctrl Pts',(12.2071238028081,0.488551624369653,4.05676737776005));
#28365=CARTESIAN_POINT('Ctrl Pts',(12.2461880325859,0.265811525316043,4.37185240566124));
#28366=CARTESIAN_POINT('Ctrl Pts',(12.269346983676,0.0635166157645696,4.41534409728183));
#28367=CARTESIAN_POINT('Ctrl Pts',(12.2766006560786,9.99581421418094E-5,
4.41520820259509));
#28368=CARTESIAN_POINT('Ctrl Pts',(12.0733993439214,0.000370082491451453,
4.41602009379308));
#28369=CARTESIAN_POINT('Ctrl Pts',(12.0861504699224,-0.110559366248508,
4.41499479059613));
#28370=CARTESIAN_POINT('Ctrl Pts',(12.1148068746109,-0.361534897467509,
4.3122242613332));
#28371=CARTESIAN_POINT('Ctrl Pts',(12.1593685579871,-0.478916017555994,
3.88799699566402));
#28372=CARTESIAN_POINT('Ctrl Pts',(12.2070843940499,-0.164809627468288,
3.53659627586117));
#28373=CARTESIAN_POINT('Ctrl Pts',(12.2548002301128,0.300643979445627,3.61074632631782));
#28374=CARTESIAN_POINT('Ctrl Pts',(12.3025160661756,0.490011594032383,4.04235401475446));
#28375=CARTESIAN_POINT('Ctrl Pts',(12.3420491041118,0.274087380788525,4.36772087084377));
#28376=CARTESIAN_POINT('Ctrl Pts',(12.3656768633604,0.0675564760281007,
4.41523665186048));
#28377=CARTESIAN_POINT('Ctrl Pts',(12.3733993439214,3.32456539758746E-5,
4.41518865831861));
#28378=CARTESIAN_POINT('Origin',(3.42660065607856,0.,4.));
#28379=CARTESIAN_POINT('',(11.6766006560786,-0.000272404999166542,4.41633191892761));
#28380=CARTESIAN_POINT('',(11.7733993439214,-0.000215373091504267,4.41642415578018));
#28381=CARTESIAN_POINT('',(3.42660065607856,4.87367679877478E-13,4.415875));
#28382=CARTESIAN_POINT('Ctrl Pts',(11.6766006560786,-0.000272404999166455,
4.41633191892761));
#28383=CARTESIAN_POINT('Ctrl Pts',(11.6784836394247,-0.0166217551361539,
4.41645573239506));
#28384=CARTESIAN_POINT('Ctrl Pts',(11.6962719014584,-0.170944672110958,
4.40814899119985));
#28385=CARTESIAN_POINT('Ctrl Pts',(11.7299654421798,-0.44220355512924,4.21531660568344));
#28386=CARTESIAN_POINT('Ctrl Pts',(11.7776812782426,-0.420270357404582,
3.74450430230823));
#28387=CARTESIAN_POINT('Ctrl Pts',(11.8253971143054,-0.0123964237846327,
3.50831762943));
#28388=CARTESIAN_POINT('Ctrl Pts',(11.8731129503683,0.406861336540243,3.72365044295193));
#28389=CARTESIAN_POINT('Ctrl Pts',(11.9208287864311,0.452492071153857,4.1927593068956));
#28390=CARTESIAN_POINT('Ctrl Pts',(11.9553246883346,0.185075114683736,4.40392780377));
#28391=CARTESIAN_POINT('Ctrl Pts',(11.9739153115504,0.0236883133891,4.41635013933017));
#28392=CARTESIAN_POINT('Ctrl Pts',(11.9766006560786,0.000344603143201134,
4.41614202049347));
#28393=CARTESIAN_POINT('Ctrl Pts',(11.7733993439214,-0.000215373091504231,
4.41642415578018));
#28394=CARTESIAN_POINT('Ctrl Pts',(11.7748135191091,-0.0124870613922979,
4.41650138834433));
#28395=CARTESIAN_POINT('Ctrl Pts',(11.7921329729843,-0.162701432614141,
4.41043584391465));
#28396=CARTESIAN_POINT('Ctrl Pts',(11.8253577055472,-0.435670260442099,
4.22824690363353));
#28397=CARTESIAN_POINT('Ctrl Pts',(11.8730735416101,-0.427612859293677,
3.75699286549843));
#28398=CARTESIAN_POINT('Ctrl Pts',(11.9207893776729,-0.0268719897862959,
3.50889601812151));
#28399=CARTESIAN_POINT('Ctrl Pts',(11.9685052137357,0.398545841420554,3.71178751390968));
#28400=CARTESIAN_POINT('Ctrl Pts',(12.0162210497986,0.457972894034889,4.17934897039372));
#28401=CARTESIAN_POINT('Ctrl Pts',(12.0511857598605,0.193343073938706,4.40127740506484));
#28402=CARTESIAN_POINT('Ctrl Pts',(12.0702451912347,0.0278098881012828,
4.41627371553856));
#28403=CARTESIAN_POINT('Ctrl Pts',(12.0733993439214,0.000370082491451453,
4.41602009379308));
#28404=CARTESIAN_POINT('Origin',(3.42660065607856,0.,4.));
#28405=CARTESIAN_POINT('',(11.3766006560786,-0.000206048103233091,4.41528588740701));
#28406=CARTESIAN_POINT('',(11.4733993439214,-0.000260100423148973,4.41535533657191));
#28407=CARTESIAN_POINT('',(3.42660065607856,4.87367679877478E-13,4.415875));
#28408=CARTESIAN_POINT('Ctrl Pts',(11.3766006560786,-0.000206048103232999,
4.41528588740701));
#28409=CARTESIAN_POINT('Ctrl Pts',(11.383051967299,-0.0565815589273492,
4.41553770218085));
#28410=CARTESIAN_POINT('Ctrl Pts',(11.4054085572071,-0.251630532720247,
4.37854193442951));
#28411=CARTESIAN_POINT('Ctrl Pts',(11.4436704258028,-0.485070265991237,
4.08131458604192));
#28412=CARTESIAN_POINT('Ctrl Pts',(11.4913862618656,-0.330742172127369,
3.63597412121053));
#28413=CARTESIAN_POINT('Ctrl Pts',(11.5391020979284,0.127311547523522,3.52492422212962));
#28414=CARTESIAN_POINT('Ctrl Pts',(11.5868179339912,0.468453114143607,3.85014371984754));
#28415=CARTESIAN_POINT('Ctrl Pts',(11.632650786708,0.382920955827079,4.29471395365306));
#28416=CARTESIAN_POINT('Ctrl Pts',(11.6625783607371,0.121478760105588,4.41540989855421));
#28417=CARTESIAN_POINT('Ctrl Pts',(11.6766006560786,-0.000272404999166455,
4.41633191892761));
#28418=CARTESIAN_POINT('Ctrl Pts',(11.4733993439214,-0.000260100423148869,
4.41535533657191));
#28419=CARTESIAN_POINT('Ctrl Pts',(11.4793818469834,-0.0525169974224216,
4.41565306322741));
#28420=CARTESIAN_POINT('Ctrl Pts',(11.501269628733,-0.243338890257842,4.3822327073369));
#28421=CARTESIAN_POINT('Ctrl Pts',(11.5390626891702,-0.482464979911041,
4.09556551685319));
#28422=CARTESIAN_POINT('Ctrl Pts',(11.586778525233,-0.341319923258817,3.64587299617429));
#28423=CARTESIAN_POINT('Ctrl Pts',(11.6344943612959,0.113264470804062,3.5213807520529));
#28424=CARTESIAN_POINT('Ctrl Pts',(11.6822101973587,0.463836358529674,3.83641192782507));
#28425=CARTESIAN_POINT('Ctrl Pts',(11.7285118582339,0.390694138047139,4.28787953265104));
#28426=CARTESIAN_POINT('Ctrl Pts',(11.7589082404215,0.125533053862222,4.41563275094549));
#28427=CARTESIAN_POINT('Ctrl Pts',(11.7733993439214,-0.000215373091504231,
4.41642415578018));
#28428=CARTESIAN_POINT('Origin',(3.42660065607856,0.,4.));
#28429=CARTESIAN_POINT('',(11.0766006560786,0.000352537510456688,4.41557576695298));
#28430=CARTESIAN_POINT('',(11.1733993439214,0.000319650745578964,4.41547275084625));
#28431=CARTESIAN_POINT('',(3.42660065607856,4.87367679877478E-13,4.415875));
#28432=CARTESIAN_POINT('Ctrl Pts',(11.0766006560786,0.000352537510456667,
4.41557576695298));
#28433=CARTESIAN_POINT('Ctrl Pts',(11.0876202951733,-0.0957751134661499,
4.41480617263661));
#28434=CARTESIAN_POINT('Ctrl Pts',(11.1145452129557,-0.331820540820521,
4.33374203885914));
#28435=CARTESIAN_POINT('Ctrl Pts',(11.1573754094257,-0.488245699001722,
3.94065893278431));
#28436=CARTESIAN_POINT('Ctrl Pts',(11.2050912454886,-0.214150733603143,
3.55723066033293));
#28437=CARTESIAN_POINT('Ctrl Pts',(11.2528070815514,0.256602145595791,3.58040428537983));
#28438=CARTESIAN_POINT('Ctrl Pts',(11.3005229176142,0.491713326162588,3.98889911147238));
#28439=CARTESIAN_POINT('Ctrl Pts',(11.3417874424566,0.304539430122629,4.35098016691413));
#28440=CARTESIAN_POINT('Ctrl Pts',(11.3671466886114,0.0824085130402235,
4.41491686960609));
#28441=CARTESIAN_POINT('Ctrl Pts',(11.3766006560786,-0.000206048103232999,
4.41528588740701));
#28442=CARTESIAN_POINT('Ctrl Pts',(11.1733993439214,0.000319650745578978,
4.41547275084625));
#28443=CARTESIAN_POINT('Ctrl Pts',(11.1839501748577,-0.0917759901056567,
4.4148158243975));
#28444=CARTESIAN_POINT('Ctrl Pts',(11.2104062844816,-0.32368545017211,4.33911969104981));
#28445=CARTESIAN_POINT('Ctrl Pts',(11.2527676727932,-0.489781601228288,
3.95506440219344));
#28446=CARTESIAN_POINT('Ctrl Pts',(11.300483508856,-0.227098200695192,3.56372986339542));
#28447=CARTESIAN_POINT('Ctrl Pts',(11.3481993449188,0.244132971891272,3.57302890392028));
#28448=CARTESIAN_POINT('Ctrl Pts',(11.3959151809817,0.491173079921361,3.97442207176994));
#28449=CARTESIAN_POINT('Ctrl Pts',(11.4376485139825,0.312739912806573,4.34603313379779));
#28450=CARTESIAN_POINT('Ctrl Pts',(11.4634765682958,0.0864149014017155,
4.41486151738456));
#28451=CARTESIAN_POINT('Ctrl Pts',(11.4733993439214,-0.000260100423148869,
4.41535533657191));
#28452=CARTESIAN_POINT('Origin',(3.42660065607856,0.,4.));
#28453=CARTESIAN_POINT('',(10.7766006560786,5.16128798610187E-5,4.41655360457584));
#28454=CARTESIAN_POINT('',(10.8733993439214,0.000125523266313186,4.41651574507477));
#28455=CARTESIAN_POINT('',(3.42660065607856,4.87367679877478E-13,4.415875));
#28456=CARTESIAN_POINT('Ctrl Pts',(10.7766006560786,5.16128798610299E-5,
4.41655360457584));
#28457=CARTESIAN_POINT('Ctrl Pts',(10.7921886230477,-0.135103241057852,
4.41631783152902));
#28458=CARTESIAN_POINT('Ctrl Pts',(10.8236818687044,-0.408598944994929,
4.27108057505162));
#28459=CARTESIAN_POINT('Ctrl Pts',(10.8710803930487,-0.451470021714238,
3.80485891169382));
#28460=CARTESIAN_POINT('Ctrl Pts',(10.9187962291115,-0.080036233235122,
3.51471716883706));
#28461=CARTESIAN_POINT('Ctrl Pts',(10.9665120651743,0.364896059739551,3.6702181168734));
#28462=CARTESIAN_POINT('Ctrl Pts',(11.0142279012372,0.47473868640782,4.1285628425314));
#28463=CARTESIAN_POINT('Ctrl Pts',(11.0509240982053,0.223935965514619,4.3902602363912));
#28464=CARTESIAN_POINT('Ctrl Pts',(11.0717150164857,0.0429714521173939,
4.4159169723618));
#28465=CARTESIAN_POINT('Ctrl Pts',(11.0766006560786,0.000352537510456667,
4.41557576695298));
#28466=CARTESIAN_POINT('Ctrl Pts',(10.8733993439214,0.000125523266313226,
4.41651574507477));
#28467=CARTESIAN_POINT('Ctrl Pts',(10.888518502732,-0.130996444363694,4.41599591363288));
#28468=CARTESIAN_POINT('Ctrl Pts',(10.9195429402303,-0.400997532511054,
4.27840016053723));
#28469=CARTESIAN_POINT('Ctrl Pts',(10.9664726564161,-0.45702143577077,3.81824018018824));
#28470=CARTESIAN_POINT('Ctrl Pts',(11.014188492479,-0.0942939790271268,
3.51728489730359));
#28471=CARTESIAN_POINT('Ctrl Pts',(11.0619043285418,0.355025089556487,3.65961432075161));
#28472=CARTESIAN_POINT('Ctrl Pts',(11.1096201646047,0.478319155637209,4.11452515096033));
#28473=CARTESIAN_POINT('Ctrl Pts',(11.1467851697312,0.23222845252417,4.38693182090163));
#28474=CARTESIAN_POINT('Ctrl Pts',(11.1680448961701,0.0470573247768451,
4.41580613485813));
#28475=CARTESIAN_POINT('Ctrl Pts',(11.1733993439214,0.000319650745578978,
4.41547275084625));
#28476=CARTESIAN_POINT('Origin',(3.42660065607856,0.,4.));
#28477=CARTESIAN_POINT('',(10.4766006560786,-0.000378910032885682,4.4157309619862));
#28478=CARTESIAN_POINT('',(10.5733993439214,-0.000383826598418624,4.41585315377736));
#28479=CARTESIAN_POINT('',(3.42660065607856,4.87367679877478E-13,4.415875));
#28480=CARTESIAN_POINT('Ctrl Pts',(10.4766006560786,-0.000378910032885704,
4.4157309619862));
#28481=CARTESIAN_POINT('Ctrl Pts',(10.4808516722344,-0.0374267536145521,
4.41605913507464));
#28482=CARTESIAN_POINT('Ctrl Pts',(10.5010079670778,-0.212714974368116,
4.3945277200383));
#28483=CARTESIAN_POINT('Ctrl Pts',(10.5370695406088,-0.469236294399976,
4.14738563318641));
#28484=CARTESIAN_POINT('Ctrl Pts',(10.5847853766716,-0.377752434501872,
3.68502647241413));
#28485=CARTESIAN_POINT('Ctrl Pts',(10.6325012127345,0.0606272984676223,
3.51191234851464));
#28486=CARTESIAN_POINT('Ctrl Pts',(10.6802170487973,0.443332050383407,3.78701662516801));
#28487=CARTESIAN_POINT('Ctrl Pts',(10.7279328848602,0.418918158891686,4.25770681210006));
#28488=CARTESIAN_POINT('Ctrl Pts',(10.7600607539539,0.143455624352724,4.41528584951654));
#28489=CARTESIAN_POINT('Ctrl Pts',(10.7762833443601,0.00280285164340033,
4.41655840401831));
#28490=CARTESIAN_POINT('Ctrl Pts',(10.7766006560786,5.16128798610299E-5,
4.41655360457584));
#28491=CARTESIAN_POINT('Ctrl Pts',(10.5733993439214,-0.000383826598418617,
4.41585315377736));
#28492=CARTESIAN_POINT('Ctrl Pts',(10.5771815519187,-0.0333213161677604,
4.41615637378185));
#28493=CARTESIAN_POINT('Ctrl Pts',(10.5968690386037,-0.20443114816448,4.39750812937281));
#28494=CARTESIAN_POINT('Ctrl Pts',(10.6324618039763,-0.464691964107356,
4.16114156306187));
#28495=CARTESIAN_POINT('Ctrl Pts',(10.6801776400391,-0.386865111317189,
3.69628860657276));
#28496=CARTESIAN_POINT('Ctrl Pts',(10.7278934761019,0.0462259258804368,
3.51033849586834));
#28497=CARTESIAN_POINT('Ctrl Pts',(10.7756093121648,0.436866984064762,3.77405207881873));
#28498=CARTESIAN_POINT('Ctrl Pts',(10.8233251482276,0.426326368719826,4.24525711444552));
#28499=CARTESIAN_POINT('Ctrl Pts',(10.8559218254798,0.151674250044741,4.4132974389186));
#28500=CARTESIAN_POINT('Ctrl Pts',(10.8726132240444,0.00694320316194716,
4.41654277368359));
#28501=CARTESIAN_POINT('Ctrl Pts',(10.8733993439214,0.000125523266313226,
4.41651574507477));
#28502=CARTESIAN_POINT('Origin',(3.42660065607856,0.,4.));
#28503=CARTESIAN_POINT('',(10.1766006560786,0.000123197149224082,4.41521991402453));
#28504=CARTESIAN_POINT('',(10.2733993439214,5.7336166378985E-5,4.41519339896199));
#28505=CARTESIAN_POINT('',(3.42660065607856,4.87367679877478E-13,4.415875));
#28506=CARTESIAN_POINT('Ctrl Pts',(10.1766006560786,0.000123197149224097,
4.41521991402453));
#28507=CARTESIAN_POINT('Ctrl Pts',(10.1854200001087,-0.0769762270984491,
4.41501595190525));
#28508=CARTESIAN_POINT('Ctrl Pts',(10.2101446228264,-0.293404201931947,
4.35739193013711));
#28509=CARTESIAN_POINT('Ctrl Pts',(10.2507745242318,-0.491764996345908,
4.00850959581219));
#28510=CARTESIAN_POINT('Ctrl Pts',(10.2984903602946,-0.273124940234581,
3.59096700393021));
#28511=CARTESIAN_POINT('Ctrl Pts',(10.3462061963575,0.196329951061554,3.54904570612073));
#28512=CARTESIAN_POINT('Ctrl Pts',(10.3939220324203,0.485492027373267,3.92124267520431));
#28513=CARTESIAN_POINT('Ctrl Pts',(10.4373868523273,0.34277731801193,4.32616121393696));
#28514=CARTESIAN_POINT('Ctrl Pts',(10.4649463935468,0.101188639822117,4.41483126760997));
#28515=CARTESIAN_POINT('Ctrl Pts',(10.4766006560786,-0.000378910032885704,
4.4157309619862));
#28516=CARTESIAN_POINT('Ctrl Pts',(10.2733993439214,5.73361663789851E-5,
4.41519339896199));
#28517=CARTESIAN_POINT('Ctrl Pts',(10.2817498797931,-0.0729553575157724,
4.41510384014646));
#28518=CARTESIAN_POINT('Ctrl Pts',(10.3060056943524,-0.285157432566911,
4.36192175935665));
#28519=CARTESIAN_POINT('Ctrl Pts',(10.3461667875993,-0.491301045992024,
4.02298928139638));
#28520=CARTESIAN_POINT('Ctrl Pts',(10.3938826236621,-0.285053227451061,
3.599188470261));
#28521=CARTESIAN_POINT('Ctrl Pts',(10.4415984597249,0.182963355965895,3.54345905416307));
#28522=CARTESIAN_POINT('Ctrl Pts',(10.4893142957878,0.482961874346273,3.9069782134126));
#28523=CARTESIAN_POINT('Ctrl Pts',(10.5332479238533,0.35082465130295,4.32033516829581));
#28524=CARTESIAN_POINT('Ctrl Pts',(10.5612762732311,0.105190355120073,4.41488124595214));
#28525=CARTESIAN_POINT('Ctrl Pts',(10.5733993439214,-0.000383826598418617,
4.41585315377736));
#28526=CARTESIAN_POINT('Origin',(3.42660065607856,0.,4.));
#28527=CARTESIAN_POINT('',(9.87660065607859,0.000332404019580576,4.41618417038907));
#28528=CARTESIAN_POINT('',(9.9733993439214,0.000362444897862246,4.41606425076498));
#28529=CARTESIAN_POINT('',(3.42660065607856,4.87367679877478E-13,4.415875));
#28530=CARTESIAN_POINT('Ctrl Pts',(9.87660065607859,0.000332404019580564,
4.41618417038907));
#28531=CARTESIAN_POINT('Ctrl Pts',(9.88998832798303,-0.116016130490024,
4.41516972706101));
#28532=CARTESIAN_POINT('Ctrl Pts',(9.91928127857509,-0.372296869871387,
4.30364082544554));
#28533=CARTESIAN_POINT('Ctrl Pts',(9.96447950785476,-0.474054618562381,
3.8689372536849));
#28534=CARTESIAN_POINT('Ctrl Pts',(10.0121953439176,-0.146148770628728,
3.53037700046135));
#28535=CARTESIAN_POINT('Ctrl Pts',(10.0599111799804,0.315967742161179,3.62307877379278));
#28536=CARTESIAN_POINT('Ctrl Pts',(10.1076270160433,0.487926215535836,4.06191310882887));
#28537=CARTESIAN_POINT('Ctrl Pts',(10.146523508076,0.262848409674369,4.37329037489646));
#28538=CARTESIAN_POINT('Ctrl Pts',(10.1695147214211,0.062069015396409,4.41538378814543));
#28539=CARTESIAN_POINT('Ctrl Pts',(10.1766006560786,0.000123197149224097,
4.41521991402453));
#28540=CARTESIAN_POINT('Ctrl Pts',(9.9733993439214,0.000362444897862267,
4.41606425076498));
#28541=CARTESIAN_POINT('Ctrl Pts',(9.9863182076674,-0.111995531308361,4.41503480155798));
#28542=CARTESIAN_POINT('Ctrl Pts',(10.015142350101,-0.364380386131072,4.30999810797653));
#28543=CARTESIAN_POINT('Ctrl Pts',(10.0598717712222,-0.477709011270712,
3.88295588266498));
#28544=CARTESIAN_POINT('Ctrl Pts',(10.1075876072851,-0.159916626226494,
3.53488507064564));
#28545=CARTESIAN_POINT('Ctrl Pts',(10.1553034433479,0.304729657315094,3.61393645496551));
#28546=CARTESIAN_POINT('Ctrl Pts',(10.2030192794107,0.489538007675758,4.04751593304174));
#28547=CARTESIAN_POINT('Ctrl Pts',(10.2423845796019,0.271127379494919,4.3692182851415));
#28548=CARTESIAN_POINT('Ctrl Pts',(10.2658446011055,0.0661120339180705,
4.41527442296197));
#28549=CARTESIAN_POINT('Ctrl Pts',(10.2733993439214,5.73361663789851E-5,
4.41519339896199));
#28550=CARTESIAN_POINT('Origin',(3.42660065607856,0.,4.));
#28551=CARTESIAN_POINT('',(9.57660065607859,-0.000290304052950346,4.41629504206998));
#28552=CARTESIAN_POINT('',(9.6733993439214,-0.000236899196693507,4.41639317328699));
#28553=CARTESIAN_POINT('',(3.42660065607856,4.87367679877478E-13,4.415875));
#28554=CARTESIAN_POINT('Ctrl Pts',(9.57660065607859,-0.000290304052950335,
4.41629504206998));
#28555=CARTESIAN_POINT('Ctrl Pts',(9.57865137716975,-0.0181001948149981,
4.41643644713422));
#28556=CARTESIAN_POINT('Ctrl Pts',(9.59660737694851,-0.173896467062472,
4.40729888742394));
#28557=CARTESIAN_POINT('Ctrl Pts',(9.63046865541489,-0.444448234747017,
4.21064422964382));
#28558=CARTESIAN_POINT('Ctrl Pts',(9.67818449147773,-0.41755432743774,3.74008922975375));
#28559=CARTESIAN_POINT('Ctrl Pts',(9.72590032754057,-0.00721385634321597,
3.50821428942208));
#28560=CARTESIAN_POINT('Ctrl Pts',(9.77361616360341,0.40975121003073,3.72795373420991));
#28561=CARTESIAN_POINT('Ctrl Pts',(9.82133199966624,0.450435435400681,4.19751745084266));
#28562=CARTESIAN_POINT('Ctrl Pts',(9.85566016382464,0.182118884769847,4.40484283743537));
#28563=CARTESIAN_POINT('Ctrl Pts',(9.87408304929542,0.0222122246324328,
4.41637494063069));
#28564=CARTESIAN_POINT('Ctrl Pts',(9.87660065607859,0.000332404019580564,
4.41618417038907));
#28565=CARTESIAN_POINT('Ctrl Pts',(9.6733993439214,-0.00023689919669354,
4.41639317328699));
#28566=CARTESIAN_POINT('Ctrl Pts',(9.67498125685411,-0.0139668454918635,
4.4164864708936));
#28567=CARTESIAN_POINT('Ctrl Pts',(9.69246844847443,-0.165649677201134,
4.40963259460397));
#28568=CARTESIAN_POINT('Ctrl Pts',(9.72586091878235,-0.438051576325333,
4.22364266437974));
#28569=CARTESIAN_POINT('Ctrl Pts',(9.77357675484519,-0.425028039486299,
3.75249971615691));
#28570=CARTESIAN_POINT('Ctrl Pts',(9.82129259090803,-0.0216947140899849,
3.50864008686857));
#28571=CARTESIAN_POINT('Ctrl Pts',(9.86900842697087,0.401561201071248,3.7160038263529));
#28572=CARTESIAN_POINT('Ctrl Pts',(9.91672426303371,0.456057286475463,4.18416562194019));
#28573=CARTESIAN_POINT('Ctrl Pts',(9.95152123535055,0.190383912560376,4.40224154849284));
#28574=CARTESIAN_POINT('Ctrl Pts',(9.97041292897978,0.0263359008882403,
4.4163022254471));
#28575=CARTESIAN_POINT('Ctrl Pts',(9.9733993439214,0.000362444897862267,
4.41606425076498));
#28576=CARTESIAN_POINT('Origin',(3.42660065607856,0.,4.));
#28577=CARTESIAN_POINT('',(9.27660065607858,-0.000185084181660103,4.41526520375254));
#28578=CARTESIAN_POINT('',(9.37339934392141,-0.000241596553487405,4.41532857883968));
#28579=CARTESIAN_POINT('',(3.42660065607856,4.87367679877478E-13,4.415875));
#28580=CARTESIAN_POINT('Ctrl Pts',(9.27660065607858,-0.000185084181660189,
4.41526520375254));
#28581=CARTESIAN_POINT('Ctrl Pts',(9.28321970504406,-0.0580335922681754,
4.4154966095816));
#28582=CARTESIAN_POINT('Ctrl Pts',(9.30574403269715,-0.254596444523232,
4.37718269734299));
#28583=CARTESIAN_POINT('Ctrl Pts',(9.34417363903789,-0.485900307124067,
4.07619787653679));
#28584=CARTESIAN_POINT('Ctrl Pts',(9.39188947510068,-0.326887306273347,
3.63250862071426));
#28585=CARTESIAN_POINT('Ctrl Pts',(9.43960531116356,0.13231133773591,3.52629235307153));
#28586=CARTESIAN_POINT('Ctrl Pts',(9.48732114722637,0.470006444430667,3.85508910653225));
#28587=CARTESIAN_POINT('Ctrl Pts',(9.53298626219807,0.380123833963086,4.29710958399465));
#28588=CARTESIAN_POINT('Ctrl Pts',(9.56274609848214,0.120032327051623,4.41533971732329));
#28589=CARTESIAN_POINT('Ctrl Pts',(9.57660065607859,-0.000290304052950335,
4.41629504206998));
#28590=CARTESIAN_POINT('Ctrl Pts',(9.3733993439214,-0.000241596553487357,
4.41532857883968));
#28591=CARTESIAN_POINT('Ctrl Pts',(9.37954958472843,-0.0539723465869793,
4.41561177485228));
#28592=CARTESIAN_POINT('Ctrl Pts',(9.40160510422307,-0.246305905820531,
4.3809303471886));
#28593=CARTESIAN_POINT('Ctrl Pts',(9.43956590240532,-0.483445357410111,
4.09047547319903));
#28594=CARTESIAN_POINT('Ctrl Pts',(9.48728173846818,-0.337568794959357,
3.64229546617122));
#28595=CARTESIAN_POINT('Ctrl Pts',(9.53499757453099,0.118302386066128,3.5226010365501));
#28596=CARTESIAN_POINT('Ctrl Pts',(9.58271341059386,0.465534665650901,3.84130942079228));
#28597=CARTESIAN_POINT('Ctrl Pts',(9.62884733372396,0.387920650713885,4.29034844530944));
#28598=CARTESIAN_POINT('Ctrl Pts',(9.65907597816649,0.124080336294106,4.41554841393524));
#28599=CARTESIAN_POINT('Ctrl Pts',(9.6733993439214,-0.00023689919669354,
4.41639317328699));
#28600=CARTESIAN_POINT('Origin',(3.42660065607856,0.,4.));
#28601=CARTESIAN_POINT('',(8.97660065607858,0.000361621133123973,4.41561526113518));
#28602=CARTESIAN_POINT('',(9.0733993439214,0.00033264130393823,4.41550825894961));
#28603=CARTESIAN_POINT('',(3.42660065607856,4.87367679877478E-13,4.415875));
#28604=CARTESIAN_POINT('Ctrl Pts',(8.97660065607858,0.000361621133123963,
4.41561526113518));
#28605=CARTESIAN_POINT('Ctrl Pts',(8.98778803291839,-0.097205817696177,
4.41480833810253));
#28606=CARTESIAN_POINT('Ctrl Pts',(9.01488068844582,-0.334723089553266,
4.33177224018802));
#28607=CARTESIAN_POINT('Ctrl Pts',(9.05787862266083,-0.487593182843731,
3.93551656882348));
#28608=CARTESIAN_POINT('Ctrl Pts',(9.10559445872368,-0.209472459465777,
3.55499829935456));
#28609=CARTESIAN_POINT('Ctrl Pts',(9.15331029478651,0.261010046587687,3.58313193881964));
#28610=CARTESIAN_POINT('Ctrl Pts',(9.20102613084934,0.491803010703882,3.99408193320625));
#28611=CARTESIAN_POINT('Ctrl Pts',(9.24212291794672,0.301599829163518,4.35270650246492));
#28612=CARTESIAN_POINT('Ctrl Pts',(9.26731442635645,0.0809737859182142,
4.41494055172187));
#28613=CARTESIAN_POINT('Ctrl Pts',(9.27660065607858,-0.000185084181660189,
4.41526520375254));
#28614=CARTESIAN_POINT('Ctrl Pts',(9.0733993439214,0.000332641303938268,
4.41550825894961));
#28615=CARTESIAN_POINT('Ctrl Pts',(9.08411791260276,-0.093207009794584,
4.4148098083896));
#28616=CARTESIAN_POINT('Ctrl Pts',(9.11074175997173,-0.326599857706223,
4.33721709571948));
#28617=CARTESIAN_POINT('Ctrl Pts',(9.1532708860283,-0.489280820139143,3.94990505119329));
#28618=CARTESIAN_POINT('Ctrl Pts',(9.20098672209113,-0.222487703095825,
3.56136068709803));
#28619=CARTESIAN_POINT('Ctrl Pts',(9.24870255815399,0.248619295113741,3.57562555337399));
#28620=CARTESIAN_POINT('Ctrl Pts',(9.29641839421681,0.49141536912078,3.97960000382683));
#28621=CARTESIAN_POINT('Ctrl Pts',(9.33798398947263,0.309808547095179,4.34782394055348));
#28622=CARTESIAN_POINT('Ctrl Pts',(9.36364430604082,0.0849819773478622,
4.41487939515448));
#28623=CARTESIAN_POINT('Ctrl Pts',(9.3733993439214,-0.000241596553487357,
4.41532857883968));
#28624=CARTESIAN_POINT('Origin',(3.42660065607856,0.,4.));
#28625=CARTESIAN_POINT('',(8.67660065607859,2.43999233753954E-5,4.41655967853978));
#28626=CARTESIAN_POINT('',(8.77339934392141,9.9565801791445E-5,4.41653262406943));
#28627=CARTESIAN_POINT('',(3.42660065607856,4.87367679877478E-13,4.415875));
#28628=CARTESIAN_POINT('Ctrl Pts',(8.67660065607859,2.43999233753836E-5,
4.41655967853978));
#28629=CARTESIAN_POINT('Ctrl Pts',(8.69235636079272,-0.136579453435425,
4.41644398151286));
#28630=CARTESIAN_POINT('Ctrl Pts',(8.72401734419445,-0.411298873006737,
4.26841067400337));
#28631=CARTESIAN_POINT('Ctrl Pts',(8.7715836062838,-0.449388340942622,3.80011167148426));
#28632=CARTESIAN_POINT('Ctrl Pts',(8.81929944234665,-0.0749173544856965,
3.51390061216986));
#28633=CARTESIAN_POINT('Ctrl Pts',(8.86701527840948,0.368351391347115,3.67408210030036));
#28634=CARTESIAN_POINT('Ctrl Pts',(8.91473111447233,0.473357386691186,4.13355901061654));
#28635=CARTESIAN_POINT('Ctrl Pts',(8.95125957369535,0.220969504140389,4.39141457480799));
#28636=CARTESIAN_POINT('Ctrl Pts',(8.97188275423077,0.0415074238114615,
4.41595555392421));
#28637=CARTESIAN_POINT('Ctrl Pts',(8.97660065607858,0.000361621133123963,
4.41561526113518));
#28638=CARTESIAN_POINT('Ctrl Pts',(8.77339934392141,9.95658017914599E-5,
4.41653262406943));
#28639=CARTESIAN_POINT('Ctrl Pts',(8.78868624047708,-0.132462770989084,
4.416105976883));
#28640=CARTESIAN_POINT('Ctrl Pts',(8.81987841572037,-0.403726445587972,
4.27580529254432));
#28641=CARTESIAN_POINT('Ctrl Pts',(8.86697586965126,-0.455080472922433,
3.81343369002772));
#28642=CARTESIAN_POINT('Ctrl Pts',(8.91469170571412,-0.0892013699275644,
3.51631793453238));
#28643=CARTESIAN_POINT('Ctrl Pts',(8.96240754177693,0.358592723611288,3.66337486216116));
#28644=CARTESIAN_POINT('Ctrl Pts',(9.0101233778398,0.477085601399612,4.11955983351088));
#28645=CARTESIAN_POINT('Ctrl Pts',(9.04712064522126,0.229261233371815,4.38814011953822));
#28646=CARTESIAN_POINT('Ctrl Pts',(9.06821263391514,0.0455964315317218,
4.41584623882512));
#28647=CARTESIAN_POINT('Ctrl Pts',(9.0733993439214,0.000332641303938268,
4.41550825894961));
#28648=CARTESIAN_POINT('Origin',(3.42660065607856,0.,4.));
#28649=CARTESIAN_POINT('',(8.37660065607859,-0.000374086211409503,4.41568853448753));
#28650=CARTESIAN_POINT('',(8.47339934392141,-0.000383538171196851,4.41580895574666));
#28651=CARTESIAN_POINT('',(3.42660065607856,4.87367679877478E-13,4.415875));
#28652=CARTESIAN_POINT('Ctrl Pts',(8.37660065607859,-0.000374086211409545,
4.41568853448753));
#28653=CARTESIAN_POINT('Ctrl Pts',(8.38101940997943,-0.0388937529272332,
4.41602262289185));
#28654=CARTESIAN_POINT('Ctrl Pts',(8.40134344256788,-0.215680110827853,
4.3934260635833));
#28655=CARTESIAN_POINT('Ctrl Pts',(8.43757275384394,-0.470763542849379,
4.14243212971755));
#28656=CARTESIAN_POINT('Ctrl Pts',(8.48528858990678,-0.37441192437669,3.68106280283335));
#28657=CARTESIAN_POINT('Ctrl Pts',(8.53300442596962,0.0657679253190804,
3.51257841158684));
#28658=CARTESIAN_POINT('Ctrl Pts',(8.58072026203246,0.445552077224736,3.79170076492532));
#28659=CARTESIAN_POINT('Ctrl Pts',(8.62843609809529,0.41617890091499,4.26210751092856));
#28660=CARTESIAN_POINT('Ctrl Pts',(8.66039622944401,0.140517691799823,4.41596716726027));
#28661=CARTESIAN_POINT('Ctrl Pts',(8.6764510821051,0.00132122424898086,
4.41656077688887));
#28662=CARTESIAN_POINT('Ctrl Pts',(8.67660065607859,2.43999233753836E-5,
4.41655967853978));
#28663=CARTESIAN_POINT('Ctrl Pts',(8.47339934392141,-0.000383538171196768,
4.41580895574666));
#28664=CARTESIAN_POINT('Ctrl Pts',(8.47734928966379,-0.0347911067166248,
4.41612244784963));
#28665=CARTESIAN_POINT('Ctrl Pts',(8.4972045140938,-0.207394442561863,4.39645832432586));
#28666=CARTESIAN_POINT('Ctrl Pts',(8.5329650172114,-0.466364439759318,4.15623518867385));
#28667=CARTESIAN_POINT('Ctrl Pts',(8.58068085327425,-0.383642787608637,
3.69222827230584));
#28668=CARTESIAN_POINT('Ctrl Pts',(8.62839668933707,0.0513839395061145,
3.51085286915611));
#28669=CARTESIAN_POINT('Ctrl Pts',(8.67611252539993,0.439224004328866,3.77866880275638));
#28670=CARTESIAN_POINT('Ctrl Pts',(8.72382836146275,0.42371790764641,4.24973658040369));
#28671=CARTESIAN_POINT('Ctrl Pts',(8.75625730096992,0.148732406864234,4.41402322426773));
#28672=CARTESIAN_POINT('Ctrl Pts',(8.77278096178947,0.00546194790078228,
4.41654988270631));
#28673=CARTESIAN_POINT('Ctrl Pts',(8.77339934392141,9.95658017914599E-5,
4.41653262406943));
#28674=CARTESIAN_POINT('Origin',(3.42660065607856,0.,4.));
#28675=CARTESIAN_POINT('',(8.07660065607859,0.000145957947245773,4.41523406184916));
#28676=CARTESIAN_POINT('',(8.1733993439214,8.12049300508987E-5,4.41520065480005));
#28677=CARTESIAN_POINT('',(3.42660065607856,4.87367679877478E-13,4.415875));
#28678=CARTESIAN_POINT('Ctrl Pts',(8.07660065607858,0.00014595794724577,
4.41523406184916));
#28679=CARTESIAN_POINT('Ctrl Pts',(8.08558773785375,-0.0784131624224431,
4.41498734772332));
#28680=CARTESIAN_POINT('Ctrl Pts',(8.11048009831652,-0.296350794919178,
4.35572875890285));
#28681=CARTESIAN_POINT('Ctrl Pts',(8.15127773746691,-0.491827368180951,
4.00332637343646));
#28682=CARTESIAN_POINT('Ctrl Pts',(8.19899357352975,-0.268798940774433,
3.58811123553743));
#28683=CARTESIAN_POINT('Ctrl Pts',(8.24670940959259,0.201071689948468,3.55113988776764));
#28684=CARTESIAN_POINT('Ctrl Pts',(8.29442524565542,0.486295093906121,3.92636368766143));
#28685=CARTESIAN_POINT('Ctrl Pts',(8.33772232781743,0.339888039743562,4.32819890206972));
#28686=CARTESIAN_POINT('Ctrl Pts',(8.36511413129181,0.0997575609540166,
4.41482007364463));
#28687=CARTESIAN_POINT('Ctrl Pts',(8.37660065607859,-0.000374086211409545,
4.41568853448753));
#28688=CARTESIAN_POINT('Ctrl Pts',(8.1733993439214,8.12049300509751E-5,
4.41520065480005));
#28689=CARTESIAN_POINT('Ctrl Pts',(8.18191761753811,-0.0743948540356096,
4.41507113968239));
#28690=CARTESIAN_POINT('Ctrl Pts',(8.20634116984244,-0.288109900049694,
4.36032095112539));
#28691=CARTESIAN_POINT('Ctrl Pts',(8.24667000083438,-0.491516046133,4.01781014446235));
#28692=CARTESIAN_POINT('Ctrl Pts',(8.29438583689722,-0.280813212199106,
3.59620653211525));
#28693=CARTESIAN_POINT('Ctrl Pts',(8.34210167296004,0.187764715363875,3.54541267448783));
#28694=CARTESIAN_POINT('Ctrl Pts',(8.38981750902289,0.483915415676709,3.91207335260334));
#28695=CARTESIAN_POINT('Ctrl Pts',(8.43358339934334,0.347950231939931,4.32244196179047));
#28696=CARTESIAN_POINT('Ctrl Pts',(8.46144401097618,0.1037581297464,4.41486010664565));
#28697=CARTESIAN_POINT('Ctrl Pts',(8.47339934392141,-0.000383538171196768,
4.41580895574666));
#28698=CARTESIAN_POINT('Origin',(3.42660065607856,0.,4.));
#28699=CARTESIAN_POINT('',(7.77660065607858,0.000318631424802313,4.41622521972442));
#28700=CARTESIAN_POINT('',(7.8733993439214,0.000353153796088606,4.4161078667978));
#28701=CARTESIAN_POINT('',(3.42660065607856,4.87367679877478E-13,4.415875));
#28702=CARTESIAN_POINT('Ctrl Pts',(7.77660065607859,0.000318631424802297,
4.41622521972442));
#28703=CARTESIAN_POINT('Ctrl Pts',(7.79015606572807,-0.117457481003694,
4.41522659035305));
#28704=CARTESIAN_POINT('Ctrl Pts',(7.81961675406517,-0.375115671948731,
4.30131743988157));
#28705=CARTESIAN_POINT('Ctrl Pts',(7.86498272108989,-0.472647010158531,
3.86394843388276));
#28706=CARTESIAN_POINT('Ctrl Pts',(7.91269855715272,-0.141191260335066,
3.52886280888004));
#28707=CARTESIAN_POINT('Ctrl Pts',(7.96041439321556,0.31992259635559,3.62642971585976));
#28708=CARTESIAN_POINT('Ctrl Pts',(8.0081302292784,0.48724661017382,4.0670519628834));
#28709=CARTESIAN_POINT('Ctrl Pts',(8.04685898356608,0.259884401562094,4.37470733986759));
#28710=CARTESIAN_POINT('Ctrl Pts',(8.06968245916614,0.0606202562326388,
4.41542398077349));
#28711=CARTESIAN_POINT('Ctrl Pts',(8.07660065607858,0.00014595794724577,
4.41523406184916));
#28712=CARTESIAN_POINT('Ctrl Pts',(7.8733993439214,0.000353153796088627,
4.4161078667978));
#28713=CARTESIAN_POINT('Ctrl Pts',(7.88648594541244,-0.113432877329791,
4.41507910421771));
#28714=CARTESIAN_POINT('Ctrl Pts',(7.9154778255911,-0.367219156371593,4.30774647947464));
#28715=CARTESIAN_POINT('Ctrl Pts',(7.96037498445733,-0.476448943335793,
3.87792777037096));
#28716=CARTESIAN_POINT('Ctrl Pts',(8.0080908205202,-0.1550058622045,3.53322552818936));
#28717=CARTESIAN_POINT('Ctrl Pts',(8.05580665658301,0.308781487260178,3.61716946571973));
#28718=CARTESIAN_POINT('Ctrl Pts',(8.10352249264587,0.489010045760349,4.0526725734847));
#28719=CARTESIAN_POINT('Ctrl Pts',(8.14272005509199,0.26816615642074,4.37069430501912));
#28720=CARTESIAN_POINT('Ctrl Pts',(8.1660123388505,0.064666477720629,4.4153129696744));
#28721=CARTESIAN_POINT('Ctrl Pts',(8.1733993439214,8.12049300509751E-5,
4.41520065480005));
#28722=CARTESIAN_POINT('Origin',(3.42660065607856,0.,4.));
#28723=CARTESIAN_POINT('',(7.47660065607859,-0.000306770237538029,4.41625647512786));
#28724=CARTESIAN_POINT('',(7.5733993439214,-0.000257198714157858,4.41635988094829));
#28725=CARTESIAN_POINT('',(3.42660065607856,4.87367679877478E-13,4.415875));
#28726=CARTESIAN_POINT('Ctrl Pts',(7.47660065607859,-0.00030677023753798,
4.41625647512786));
#28727=CARTESIAN_POINT('Ctrl Pts',(7.47881911491479,-0.0195780710793754,
4.41641565502598));
#28728=CARTESIAN_POINT('Ctrl Pts',(7.4969428524386,-0.176849480241104,4.4064317922735));
#28729=CARTESIAN_POINT('Ctrl Pts',(7.53097186865002,-0.44664354691983,4.20594845626764));
#28730=CARTESIAN_POINT('Ctrl Pts',(7.57868770471286,-0.414791917646955,
3.73570302684109));
#28731=CARTESIAN_POINT('Ctrl Pts',(7.62640354077569,-0.00203048755240202,
3.50816557464413));
#28732=CARTESIAN_POINT('Ctrl Pts',(7.67411937683853,0.412595570264971,3.73228724307244));
#28733=CARTESIAN_POINT('Ctrl Pts',(7.72183521290137,0.448328767436039,4.20225365549051));
#28734=CARTESIAN_POINT('Ctrl Pts',(7.75599563931472,0.179163779268806,4.40574053813273));
#28735=CARTESIAN_POINT('Ctrl Pts',(7.77425078704046,0.0207354574140521,
4.41639833498254));
#28736=CARTESIAN_POINT('Ctrl Pts',(7.77660065607859,0.000318631424802297,
4.41622521972442));
#28737=CARTESIAN_POINT('Ctrl Pts',(7.5733993439214,-0.000257198714157839,
4.41635988094829));
#28738=CARTESIAN_POINT('Ctrl Pts',(7.57514899459915,-0.0154461882200338,
4.41646996636401));
#28739=CARTESIAN_POINT('Ctrl Pts',(7.59280392396451,-0.168599214901356,
4.40881268721627));
#28740=CARTESIAN_POINT('Ctrl Pts',(7.62636413201748,-0.440384235482588,
4.21901358396786));
#28741=CARTESIAN_POINT('Ctrl Pts',(7.67407996808031,-0.422396009600076,
3.7480340579683));
#28742=CARTESIAN_POINT('Ctrl Pts',(7.72179580414317,-0.0165150286377962,
3.50843873354525));
#28743=CARTESIAN_POINT('Ctrl Pts',(7.76951164020598,0.404531957204003,3.72025168374225));
#28744=CARTESIAN_POINT('Ctrl Pts',(7.81722747626884,0.454091022239626,4.18896181724392));
#28745=CARTESIAN_POINT('Ctrl Pts',(7.85185671084063,0.187425762196077,4.40318800700955));
#28746=CARTESIAN_POINT('Ctrl Pts',(7.87058066672482,0.02486112795907,4.41632944836175));
#28747=CARTESIAN_POINT('Ctrl Pts',(7.8733993439214,0.000353153796088627,
4.4161078667978));
#28748=CARTESIAN_POINT('Origin',(3.42660065607856,0.,4.));
#28749=CARTESIAN_POINT('',(7.17660065607858,-0.000163391746992416,4.4152468210878));
#28750=CARTESIAN_POINT('',(7.2733993439214,-0.000222139526412562,4.4153039283715));
#28751=CARTESIAN_POINT('',(3.42660065607856,4.87367679877478E-13,4.415875));
#28752=CARTESIAN_POINT('Ctrl Pts',(7.17660065607859,-0.000163391746992363,
4.4152468210878));
#28753=CARTESIAN_POINT('Ctrl Pts',(7.18338744278911,-0.0594844418834033,
4.41545575762517));
#28754=CARTESIAN_POINT('Ctrl Pts',(7.20607950818724,-0.257561782965025,
4.37580284351512));
#28755=CARTESIAN_POINT('Ctrl Pts',(7.24467685227299,-0.486676365692783,
4.07107270446015));
#28756=CARTESIAN_POINT('Ctrl Pts',(7.29239268833582,-0.322996137187983,
3.62908393881966));
#28757=CARTESIAN_POINT('Ctrl Pts',(7.34010852439867,0.137296434535941,3.52771310152703));
#28758=CARTESIAN_POINT('Ctrl Pts',(7.3878243604615,0.471507566988788,3.86005058906394));
#28759=CARTESIAN_POINT('Ctrl Pts',(7.43332173768814,0.377318713751663,4.29947917201381));
#28760=CARTESIAN_POINT('Ctrl Pts',(7.46291383622717,0.118587850938607,4.41527441201542));
#28761=CARTESIAN_POINT('Ctrl Pts',(7.47660065607859,-0.00030677023753798,
4.41625647512786));
#28762=CARTESIAN_POINT('Ctrl Pts',(7.2733993439214,-0.000222139526412493,
4.4153039283715));
#28763=CARTESIAN_POINT('Ctrl Pts',(7.27971732247348,-0.0554265094472961,
4.41557047734173));
#28764=CARTESIAN_POINT('Ctrl Pts',(7.30194057971316,-0.249272617462211,
4.37960776139715));
#28765=CARTESIAN_POINT('Ctrl Pts',(7.34006911564044,-0.484372034479295,
4.08537538031203));
#28766=CARTESIAN_POINT('Ctrl Pts',(7.3877849517033,-0.333780171974684,3.63875766810317));
#28767=CARTESIAN_POINT('Ctrl Pts',(7.43550078776612,0.123327161313159,3.52387434835784));
#28768=CARTESIAN_POINT('Ctrl Pts',(7.48321662382897,0.467181263150904,3.84622454030349));
#28769=CARTESIAN_POINT('Ctrl Pts',(7.52918280921405,0.385138488472668,4.29279105563264));
#28770=CARTESIAN_POINT('Ctrl Pts',(7.55924371591154,0.122630008444172,4.41546922990911));
#28771=CARTESIAN_POINT('Ctrl Pts',(7.5733993439214,-0.000257198714157839,
4.41635988094829));
#28772=CARTESIAN_POINT('Origin',(3.42660065607856,0.,4.));
#28773=CARTESIAN_POINT('',(6.87660065607859,0.000369753976522709,4.4156559906262));
#28774=CARTESIAN_POINT('',(6.9733993439214,0.000344359613660638,4.41554532105972));
#28775=CARTESIAN_POINT('',(3.42660065607856,4.87367679877478E-13,4.415875));
#28776=CARTESIAN_POINT('Ctrl Pts',(6.87660065607859,0.000369753976522759,
4.4156559906262));
#28777=CARTESIAN_POINT('Ctrl Pts',(6.88795577066343,-0.0986361616094132,
4.41481368816743));
#28778=CARTESIAN_POINT('Ctrl Pts',(6.91521616393589,-0.337621850525623,
4.32977807754403));
#28779=CARTESIAN_POINT('Ctrl Pts',(6.95838183589596,-0.486886005735063,
3.93038141845316));
#28780=CARTESIAN_POINT('Ctrl Pts',(7.0060976719588,-0.204771183672361,3.55281534000283));
#28781=CARTESIAN_POINT('Ctrl Pts',(7.05381350802163,0.265389096458903,3.58590591031157));
#28782=CARTESIAN_POINT('Ctrl Pts',(7.10152934408448,0.491837993618785,3.99926540470374));
#28783=CARTESIAN_POINT('Ctrl Pts',(7.14245839343679,0.298657604039877,4.35441002681052));
#28784=CARTESIAN_POINT('Ctrl Pts',(7.16748216410149,0.0795383202432945,
4.41496610118));
#28785=CARTESIAN_POINT('Ctrl Pts',(7.17660065607859,-0.000163391746992363,
4.4152468210878));
#28786=CARTESIAN_POINT('Ctrl Pts',(6.9733993439214,0.00034435961366068,
4.41554532105972));
#28787=CARTESIAN_POINT('Ctrl Pts',(6.9842856503478,-0.0946377878655052,
4.41480662962373));
#28788=CARTESIAN_POINT('Ctrl Pts',(7.0110772354618,-0.329510302625179,4.33529054280597));
#28789=CARTESIAN_POINT('Ctrl Pts',(7.05377409926342,-0.488725618924084,
3.94475128051735));
#28790=CARTESIAN_POINT('Ctrl Pts',(7.10148993532626,-0.21785253135038,3.55904022429238));
#28791=CARTESIAN_POINT('Ctrl Pts',(7.14920577138909,0.253078023397415,3.57826934481931));
#28792=CARTESIAN_POINT('Ctrl Pts',(7.19692160745195,0.491603063369337,3.98478019943955));
#28793=CARTESIAN_POINT('Ctrl Pts',(7.2383194649627,0.306874094293292,4.34959156107453));
#28794=CARTESIAN_POINT('Ctrl Pts',(7.26381204378586,0.0835484619188193,
4.41489945011039));
#28795=CARTESIAN_POINT('Ctrl Pts',(7.2733993439214,-0.000222139526412493,
4.4153039283715));
#28796=CARTESIAN_POINT('Origin',(3.42660065607856,0.,4.));
#28797=CARTESIAN_POINT('',(6.57660065607858,1.8302248101926E-5,4.41656360501758));
#28798=CARTESIAN_POINT('',(6.6733993439214,7.63499956435865E-5,4.4165465803965));
#28799=CARTESIAN_POINT('',(3.42660065607856,4.87367679877478E-13,4.415875));
#28800=CARTESIAN_POINT('Ctrl Pts',(6.57660065607858,1.83022481018748E-5,
4.41656360501758));
#28801=CARTESIAN_POINT('Ctrl Pts',(6.57661881985014,-0.000139156870309867,
4.41656362372179));
#28802=CARTESIAN_POINT('Ctrl Pts',(6.59254226230931,-0.138177237712184,
4.41649399470799));
#28803=CARTESIAN_POINT('Ctrl Pts',(6.62437098345609,-0.41404349770976,4.26553045144514));
#28804=CARTESIAN_POINT('Ctrl Pts',(6.67208681951894,-0.447234019333667,
3.79538894860702));
#28805=CARTESIAN_POINT('Ctrl Pts',(6.71980265558177,-0.0698021891909718,
3.51313682319347));
#28806=CARTESIAN_POINT('Ctrl Pts',(6.76751849164461,0.371772181936036,3.67798293440124));
#28807=CARTESIAN_POINT('Ctrl Pts',(6.81523432770745,0.471920133146607,4.13853999974893));
#28808=CARTESIAN_POINT('Ctrl Pts',(6.85159504918544,0.21800401543618,4.39254992240466));
#28809=CARTESIAN_POINT('Ctrl Pts',(6.87205049197582,0.0400429038769189,
4.41599351380864));
#28810=CARTESIAN_POINT('Ctrl Pts',(6.87660065607859,0.000369753976522759,
4.4156559906262));
#28811=CARTESIAN_POINT('Ctrl Pts',(6.6733993439214,7.63499956435956E-5,
4.4165465803965));
#28812=CARTESIAN_POINT('Ctrl Pts',(6.68885397822212,-0.133927014866661,
4.41622291450327));
#28813=CARTESIAN_POINT('Ctrl Pts',(6.72021389121046,-0.406451392834186,
4.27318229388465));
#28814=CARTESIAN_POINT('Ctrl Pts',(6.76747908288639,-0.453085647428837,
3.80864864857145));
#28815=CARTESIAN_POINT('Ctrl Pts',(6.81519491894923,-0.0841006081168706,
3.51540431248109));
#28816=CARTESIAN_POINT('Ctrl Pts',(6.86291075501207,0.362121456530253,3.66717299786736));
#28817=CARTESIAN_POINT('Ctrl Pts',(6.91062659107491,0.475798562415156,4.124581128109));
#28818=CARTESIAN_POINT('Ctrl Pts',(6.94745612071136,0.226294304474162,4.38932900794447));
#28819=CARTESIAN_POINT('Ctrl Pts',(6.96838037166019,0.0441344886838037,
4.41588588393584));
#28820=CARTESIAN_POINT('Ctrl Pts',(6.9733993439214,0.00034435961366068,
4.41554532105972));
#28821=CARTESIAN_POINT('Origin',(3.42660065607856,0.,4.));
#28822=CARTESIAN_POINT('',(6.27660065607859,-8.94903747701068E-6,4.41582842213685));
#28823=CARTESIAN_POINT('',(6.3733993439214,-0.000441664590319634,4.4157663968931));
#28824=CARTESIAN_POINT('',(3.42660065607856,4.87367679877478E-13,4.415875));
#28825=CARTESIAN_POINT('Ctrl Pts',(6.27660065607859,-8.94903747701223E-6,
4.41582842213685));
#28826=CARTESIAN_POINT('Ctrl Pts',(6.28118714772447,-0.0399801639742102,
4.41579747358059));
#28827=CARTESIAN_POINT('Ctrl Pts',(6.29372627871415,-0.149263049162913,
4.40013952362907));
#28828=CARTESIAN_POINT('Ctrl Pts',(6.31421804904765,-0.307151379675736,
4.3060270879454));
#28829=CARTESIAN_POINT('Ctrl Pts',(6.33807596707907,-0.416657206472865,
4.12081787696614));
#28830=CARTESIAN_POINT('Ctrl Pts',(6.36193388511048,-0.422829889105799,
3.9075587958503));
#28831=CARTESIAN_POINT('Ctrl Pts',(6.39374444248571,-0.296437506874183,
3.64987069373525));
#28832=CARTESIAN_POINT('Ctrl Pts',(6.43350763920474,0.0703302468340302,
3.51324810367198));
#28833=CARTESIAN_POINT('Ctrl Pts',(6.48122347526758,0.448014600657906,3.7964368525222));
#28834=CARTESIAN_POINT('Ctrl Pts',(6.52892114755886,0.413253290380966,4.26628466471864));
#28835=CARTESIAN_POINT('Ctrl Pts',(6.56071354116253,0.137741412285014,4.41654724519979));
#28836=CARTESIAN_POINT('Ctrl Pts',(6.57660065607858,1.83022481018748E-5,
4.41656360501758));
#28837=CARTESIAN_POINT('Ctrl Pts',(6.3733993439214,-0.000441664590319611,
4.4157663968931));
#28838=CARTESIAN_POINT('Ctrl Pts',(6.37751702740883,-0.0362476131304844,
4.41610293027605));
#28839=CARTESIAN_POINT('Ctrl Pts',(6.39753998958387,-0.210006484715375,
4.39546152579387));
#28840=CARTESIAN_POINT('Ctrl Pts',(6.43346823044653,-0.468271923807345,
4.15124960425567));
#28841=CARTESIAN_POINT('Ctrl Pts',(6.48118406650937,-0.380227249479543,
3.6882349865083));
#28842=CARTESIAN_POINT('Ctrl Pts',(6.52889990257221,0.0564566449812287,
3.51140415777354));
#28843=CARTESIAN_POINT('Ctrl Pts',(6.57661573863504,0.441574375138847,3.78331933667001));
#28844=CARTESIAN_POINT('Ctrl Pts',(6.62433157469789,0.421040068198854,4.25418342072721));
#28845=CARTESIAN_POINT('Ctrl Pts',(6.65659277646,0.145792717270209,4.41473316952435));
#28846=CARTESIAN_POINT('Ctrl Pts',(6.6729486995345,0.00398377756883227,
4.41655601822694));
#28847=CARTESIAN_POINT('Ctrl Pts',(6.6733993439214,7.63499956435956E-5,
4.4165465803965));
#28848=CARTESIAN_POINT('Origin',(3.42660065607856,0.,4.));
#28849=CARTESIAN_POINT('',(5.97660065607859,-9.19412645702589E-6,4.41589218083175));
#28850=CARTESIAN_POINT('',(6.0733993439214,-6.65563173402051E-6,4.41590255337155));
#28851=CARTESIAN_POINT('',(3.42660065607856,4.87367679877478E-13,4.415875));
#28852=CARTESIAN_POINT('Ctrl Pts',(5.97660065607858,-9.19412645705893E-6,
4.41589218083175));
#28853=CARTESIAN_POINT('Ctrl Pts',(5.97780283625498,-0.0104787976275591,
4.4159022685469));
#28854=CARTESIAN_POINT('Ctrl Pts',(5.98695765577519,-0.0902010538040918,
4.41295272969856));
#28855=CARTESIAN_POINT('Ctrl Pts',(6.0040651146392,-0.23587461323539,4.36380751861078));
#28856=CARTESIAN_POINT('Ctrl Pts',(6.02792303267061,-0.381351759249696,
4.20630938167977));
#28857=CARTESIAN_POINT('Ctrl Pts',(6.05178095070204,-0.433578399193506,
3.9983625870902));
#28858=CARTESIAN_POINT('Ctrl Pts',(6.07563886873346,-0.379782579589031,
3.79081692866841));
#28859=CARTESIAN_POINT('Ctrl Pts',(6.09949678676487,-0.233120953551068,
3.63442082419035));
#28860=CARTESIAN_POINT('Ctrl Pts',(6.12335470479629,-0.0294522997972467,
3.5674214393556));
#28861=CARTESIAN_POINT('Ctrl Pts',(6.14721262282771,0.181413325723775,3.60619428643423));
#28862=CARTESIAN_POINT('Ctrl Pts',(6.17107054085913,0.347927737305898,3.74127281623538));
#28863=CARTESIAN_POINT('Ctrl Pts',(6.19492845889055,0.429346806292137,3.93959933010928));
#28864=CARTESIAN_POINT('Ctrl Pts',(6.21878637692197,0.405811992579865,4.15272917617017));
#28865=CARTESIAN_POINT('Ctrl Pts',(6.24264429495339,0.282982581651336,4.32844890303245));
#28866=CARTESIAN_POINT('Ctrl Pts',(6.26191572133893,0.127967070080381,4.40561019629887));
#28867=CARTESIAN_POINT('Ctrl Pts',(6.27323450838066,0.029326984292613,4.415851136102));
#28868=CARTESIAN_POINT('Ctrl Pts',(6.27660065607859,-8.94903747701223E-6,
4.41582842213685));
#28869=CARTESIAN_POINT('Ctrl Pts',(6.0733993439214,-6.65563173397714E-6,
4.41590255337156));
#28870=CARTESIAN_POINT('Ctrl Pts',(6.07413271593935,-0.00639299139291402,
4.41590724351385));
#28871=CARTESIAN_POINT('Ctrl Pts',(6.0828187273011,-0.0820297780542147,
4.41420140028919));
#28872=CARTESIAN_POINT('Ctrl Pts',(6.09945737800665,-0.2250554921608,4.3705991908187));
#28873=CARTESIAN_POINT('Ctrl Pts',(6.12331529603809,-0.375113923638194,
4.21744656883549));
#28874=CARTESIAN_POINT('Ctrl Pts',(6.1471732140695,-0.433431396087355,4.01114207710762));
#28875=CARTESIAN_POINT('Ctrl Pts',(6.17103113210093,-0.385792139046387,
3.80207577201042));
#28876=CARTESIAN_POINT('Ctrl Pts',(6.19488905013233,-0.243761337718234,
3.64147770828707));
#28877=CARTESIAN_POINT('Ctrl Pts',(6.21874696816376,-0.042227823444436,
3.56841523311022));
#28878=CARTESIAN_POINT('Ctrl Pts',(6.24260488619517,0.16982704650124,3.60113783246665));
#28879=CARTESIAN_POINT('Ctrl Pts',(6.2664628042266,0.339985970990829,3.73091992247201));
#28880=CARTESIAN_POINT('Ctrl Pts',(6.29032072225801,0.427700638223926,3.92738904240251));
#28881=CARTESIAN_POINT('Ctrl Pts',(6.31417864028943,0.409561128158778,4.13996490148311));
#28882=CARTESIAN_POINT('Ctrl Pts',(6.34187151417723,0.27471212230801,4.35031587281991));
#28883=CARTESIAN_POINT('Ctrl Pts',(6.36161174872122,0.102059178040878,4.41480301073152));
#28884=CARTESIAN_POINT('Ctrl Pts',(6.3733993439214,-0.000441664590319611,
4.4157663968931));
#28885=CARTESIAN_POINT('Origin',(3.42660065607856,0.,4.));
#28886=CARTESIAN_POINT('',(5.67660065607858,1.06631253201556E-5,4.41586554077139));
#28887=CARTESIAN_POINT('',(5.7733993439214,9.17748676071416E-6,4.4158542849441));
#28888=CARTESIAN_POINT('',(3.42660065607856,4.87367679877478E-13,4.415875));
#28889=CARTESIAN_POINT('Ctrl Pts',(5.67660065607858,1.06631253201268E-5,
4.41586554077139));
#28890=CARTESIAN_POINT('Ctrl Pts',(5.68237116412931,-0.050253077703417,
4.41581669384736));
#28891=CARTESIAN_POINT('Ctrl Pts',(5.69609431152383,-0.169828933264711,
4.3941204493343));
#28892=CARTESIAN_POINT('Ctrl Pts',(5.71777009826218,-0.329222253834466,
4.28214440376531));
#28893=CARTESIAN_POINT('Ctrl Pts',(5.74162801629359,-0.424158110434281,
4.08990358344764));
#28894=CARTESIAN_POINT('Ctrl Pts',(5.76548593432501,-0.415375755386326,
3.8756788878607));
#28895=CARTESIAN_POINT('Ctrl Pts',(5.78934385235642,-0.305022713182347,
3.69185409099321));
#28896=CARTESIAN_POINT('Ctrl Pts',(5.81320177038785,-0.120083309624962,
3.58337936191985));
#28897=CARTESIAN_POINT('Ctrl Pts',(5.83705968841926,0.0942197354074567,
3.57677972866706));
#28898=CARTESIAN_POINT('Ctrl Pts',(5.86091760645069,0.285483486244351,3.673668977605));
#28899=CARTESIAN_POINT('Ctrl Pts',(5.8847755244821,0.406938752801468,3.85035505520226));
#28900=CARTESIAN_POINT('Ctrl Pts',(5.90863344251353,0.428886400972996,4.06363338935351));
#28901=CARTESIAN_POINT('Ctrl Pts',(5.93249136054494,0.345959657594393,4.261351642888));
#28902=CARTESIAN_POINT('Ctrl Pts',(5.95514709839996,0.186877681905787,4.38841966610496));
#28903=CARTESIAN_POINT('Ctrl Pts',(5.96985019691118,0.0587795235055939,
4.41583553648629));
#28904=CARTESIAN_POINT('Ctrl Pts',(5.97660065607858,-9.19412645705893E-6,
4.41589218083175));
#28905=CARTESIAN_POINT('Ctrl Pts',(5.7733993439214,9.17748676073846E-6,
4.4158542849441));
#28906=CARTESIAN_POINT('Ctrl Pts',(5.77870104381367,-0.0461746181927863,
4.41581721944429));
#28907=CARTESIAN_POINT('Ctrl Pts',(5.79195538304975,-0.161664917198308,
4.3966319946429));
#28908=CARTESIAN_POINT('Ctrl Pts',(5.81316236162963,-0.320769768688322,
4.29171820750724));
#28909=CARTESIAN_POINT('Ctrl Pts',(5.83702027966105,-0.421326288178809,
4.10235681181338));
#28910=CARTESIAN_POINT('Ctrl Pts',(5.86087819769247,-0.418857046020503,
3.88796639709818));
#28911=CARTESIAN_POINT('Ctrl Pts',(5.88473611572389,-0.313965860818636,
3.70097123187977));
#28912=CARTESIAN_POINT('Ctrl Pts',(5.90859403375531,-0.132301443679057,
3.58709678011166));
#28913=CARTESIAN_POINT('Ctrl Pts',(5.93245195178673,0.0817142298265842,
3.57418834816524));
#28914=CARTESIAN_POINT('Ctrl Pts',(5.95630986981814,0.275748643515392,3.66540258613358));
#28915=CARTESIAN_POINT('Ctrl Pts',(5.98016778784957,0.402354822815078,3.83843477537114));
#28916=CARTESIAN_POINT('Ctrl Pts',(6.00402570588098,0.430574627524036,4.05097449853386));
#28917=CARTESIAN_POINT('Ctrl Pts',(6.02788362391241,0.353506566116634,4.25104874587108));
#28918=CARTESIAN_POINT('Ctrl Pts',(6.05100816992587,0.195023852357142,4.38547315270063));
#28919=CARTESIAN_POINT('Ctrl Pts',(6.06618007659554,0.06286002589468,4.4158563839102));
#28920=CARTESIAN_POINT('Ctrl Pts',(6.0733993439214,-6.65563173397714E-6,
4.41590255337156));
#28921=CARTESIAN_POINT('Origin',(3.42660065607856,0.,4.));
#28922=CARTESIAN_POINT('',(5.37660065607858,-1.01751121954902E-5,4.41586038335289));
#28923=CARTESIAN_POINT('',(5.4733993439214,-1.09014992595302E-5,4.41587264340464));
#28924=CARTESIAN_POINT('',(3.42660065607856,4.87367679877478E-13,4.415875));
#28925=CARTESIAN_POINT('Ctrl Pts',(5.37660065607859,-1.01751121954468E-5,
4.41586038335289));
#28926=CARTESIAN_POINT('Ctrl Pts',(5.37898685265982,-0.0207957689391596,
4.41587928195339));
#28927=CARTESIAN_POINT('Ctrl Pts',(5.38932568858487,-0.110842971866809,
4.40924760552439));
#28928=CARTESIAN_POINT('Ctrl Pts',(5.40761716385372,-0.26226226804932,4.34526983614494));
#28929=CARTESIAN_POINT('Ctrl Pts',(5.43147508188515,-0.395631058815178,
4.17739453851434));
#28930=CARTESIAN_POINT('Ctrl Pts',(5.45533299991656,-0.432257278927009,
3.96614144408682));
#28931=CARTESIAN_POINT('Ctrl Pts',(5.47919091794798,-0.363184819889405,
3.76316768886851));
#28932=CARTESIAN_POINT('Ctrl Pts',(5.5030488359794,-0.205303779432806,3.61810588490468));
#28933=CARTESIAN_POINT('Ctrl Pts',(5.52690675401082,0.00277962745745752,
3.56642759466814));
#28934=CARTESIAN_POINT('Ctrl Pts',(5.55076467204224,0.210183339719457,3.62076956781107));
#28935=CARTESIAN_POINT('Ctrl Pts',(5.57462259007365,0.36619150013966,3.76784371165257));
#28936=CARTESIAN_POINT('Ctrl Pts',(5.59848050810508,0.432655863921731,3.97168639180759));
#28937=CARTESIAN_POINT('Ctrl Pts',(5.62233842613649,0.393324083661671,4.18245252040861));
#28938=CARTESIAN_POINT('Ctrl Pts',(5.64619634416792,0.257813851021257,4.34860403787086));
#28939=CARTESIAN_POINT('Ctrl Pts',(5.66428375414861,0.107285005985459,4.40994309575933));
#28940=CARTESIAN_POINT('Ctrl Pts',(5.6744185247855,0.0190180158238588,4.41588401235146));
#28941=CARTESIAN_POINT('Ctrl Pts',(5.67660065607858,1.06631253201268E-5,
4.41586554077139));
#28942=CARTESIAN_POINT('Ctrl Pts',(5.4733993439214,-1.0901499259525E-5,
4.41587264340464));
#28943=CARTESIAN_POINT('Ctrl Pts',(5.47531673234419,-0.0167114040746605,
4.41588973972128));
#28944=CARTESIAN_POINT('Ctrl Pts',(5.48518676011079,-0.102669266038577,
4.41080986982701));
#28945=CARTESIAN_POINT('Ctrl Pts',(5.50300942722118,-0.251979671819092,
4.35284416104532));
#28946=CARTESIAN_POINT('Ctrl Pts',(5.52686734525261,-0.390234841353927,
4.18896964197264));
#28947=CARTESIAN_POINT('Ctrl Pts',(5.55072526328402,-0.433066962396004,
3.97888689800548));
#28948=CARTESIAN_POINT('Ctrl Pts',(5.57458318131544,-0.370002414621403,
3.77396688259));
#28949=CARTESIAN_POINT('Ctrl Pts',(5.59844109934686,-0.21646219781534,3.62431812139094));
#28950=CARTESIAN_POINT('Ctrl Pts',(5.62229901737828,-0.00999107731853999,
3.56653381289738));
#28951=CARTESIAN_POINT('Ctrl Pts',(5.64615693540971,0.198923133709572,3.61474379450078));
#28952=CARTESIAN_POINT('Ctrl Pts',(5.67001485344111,0.359195220034686,3.75715941257656));
#28953=CARTESIAN_POINT('Ctrl Pts',(5.69387277147254,0.431634290692432,3.95895616900985));
#28954=CARTESIAN_POINT('Ctrl Pts',(5.71773068950395,0.398527019959163,4.1707892603438));
#28955=CARTESIAN_POINT('Ctrl Pts',(5.74158860753538,0.267969036875697,4.34085972491723));
#28956=CARTESIAN_POINT('Ctrl Pts',(5.76014482567452,0.115458993192439,4.40830959117706));
#28957=CARTESIAN_POINT('Ctrl Pts',(5.77074840446986,0.0231018550196917,
4.41587281831976));
#28958=CARTESIAN_POINT('Ctrl Pts',(5.7733993439214,9.17748676073846E-6,
4.4158542849441));
#28959=CARTESIAN_POINT('Origin',(3.42660065607856,0.,4.));
#28960=CARTESIAN_POINT('',(5.07660065607859,8.10857529294212E-6,4.41589722116852));
#28961=CARTESIAN_POINT('',(5.1733993439214,1.02299162792543E-5,4.4158851107878));
#28962=CARTESIAN_POINT('',(3.42660065607856,4.87367679877478E-13,4.415875));
#28963=CARTESIAN_POINT('Ctrl Pts',(5.07660065607858,8.10857529294148E-6,
4.41589722116852));
#28964=CARTESIAN_POINT('Ctrl Pts',(5.08355518053415,-0.060555656273516,
4.41584370653314));
#28965=CARTESIAN_POINT('Ctrl Pts',(5.09846234433351,-0.190424342306974,
4.38715451669839));
#28966=CARTESIAN_POINT('Ctrl Pts',(5.1213221474767,-0.349282119693095,4.256894448863));
#28967=CARTESIAN_POINT('Ctrl Pts',(5.1451800655081,-0.4296670234643,4.05812921762123));
#28968=CARTESIAN_POINT('Ctrl Pts',(5.16903798353954,-0.404986636103755,
3.84514980926298));
#28969=CARTESIAN_POINT('Ctrl Pts',(5.19289590157095,-0.281275984601366,
3.67003549057442));
#28970=CARTESIAN_POINT('Ctrl Pts',(5.21675381960238,-0.0887856930599551,
3.5756064824932));
#28971=CARTESIAN_POINT('Ctrl Pts',(5.24061173763379,0.125415118908336,3.58495324968971));
#28972=CARTESIAN_POINT('Ctrl Pts',(5.26446965566521,0.308948518064291,3.69579025298356));
#28973=CARTESIAN_POINT('Ctrl Pts',(5.28832757369662,0.416935588964862,3.88101482593007));
#28974=CARTESIAN_POINT('Ctrl Pts',(5.31218549172805,0.422970551266107,4.09533451502773));
#28975=CARTESIAN_POINT('Ctrl Pts',(5.33604340975946,0.325577692296299,4.28634231834109));
#28976=CARTESIAN_POINT('Ctrl Pts',(5.35751513120965,0.166275769440666,4.39523064161658));
#28977=CARTESIAN_POINT('Ctrl Pts',(5.37103421331602,0.0484777907299229,
4.41581629730449));
#28978=CARTESIAN_POINT('Ctrl Pts',(5.37660065607859,-1.01751121954468E-5,
4.41586038335289));
#28979=CARTESIAN_POINT('Ctrl Pts',(5.1733993439214,1.02299162792474E-5,
4.4158851107878));
#28980=CARTESIAN_POINT('Ctrl Pts',(5.17988506021851,-0.0564756498766958,
4.41582730150705));
#28981=CARTESIAN_POINT('Ctrl Pts',(5.19432341585943,-0.182274442988225,
4.39002065289559));
#28982=CARTESIAN_POINT('Ctrl Pts',(5.21671441084416,-0.341564590845109,
4.26707000444592));
#28983=CARTESIAN_POINT('Ctrl Pts',(5.24057232887557,-0.427768622694993,
4.07075847957352));
#28984=CARTESIAN_POINT('Ctrl Pts',(5.264430246907,-0.409371574112622,3.85714457902312));
#28985=CARTESIAN_POINT('Ctrl Pts',(5.2882881649384,-0.290872024601924,3.6784627202051));
#28986=CARTESIAN_POINT('Ctrl Pts',(5.31214608296984,-0.101246341881189,
3.57840548479658));
#28987=CARTESIAN_POINT('Ctrl Pts',(5.33600400100125,0.113136829324483,3.58143959235932));
#28988=CARTESIAN_POINT('Ctrl Pts',(5.35986191903268,0.299854963974951,3.68682312094679));
#28989=CARTESIAN_POINT('Ctrl Pts',(5.38371983706408,0.413250392048343,3.8687869272297));
#28990=CARTESIAN_POINT('Ctrl Pts',(5.40757775509551,0.425594842551202,4.08283590397723));
#28991=CARTESIAN_POINT('Ctrl Pts',(5.43143567312693,0.333869761079625,4.27662924579771));
#28992=CARTESIAN_POINT('Ctrl Pts',(5.45337620273556,0.174437273907163,4.39264091290779));
#28993=CARTESIAN_POINT('Ctrl Pts',(5.46736409300038,0.0525562895569378,
4.41581883033293));
#28994=CARTESIAN_POINT('Ctrl Pts',(5.4733993439214,-1.0901499259525E-5,
4.41587264340464));
#28995=CARTESIAN_POINT('Origin',(3.42660065607856,0.,4.));
#28996=CARTESIAN_POINT('',(4.77660065607858,-3.27394476109793E-6,4.41584059078716));
#28997=CARTESIAN_POINT('',(4.8733993439214,-6.67049670156904E-6,4.4158459349409));
#28998=CARTESIAN_POINT('',(3.42660065607856,4.87367679877478E-13,4.415875));
#28999=CARTESIAN_POINT('Ctrl Pts',(4.77660065607858,-3.27394476113199E-6,
4.41584059078717));
#29000=CARTESIAN_POINT('Ctrl Pts',(4.78017086906467,-0.0311067951354469,
4.4158491206715));
#29001=CARTESIAN_POINT('Ctrl Pts',(4.79169372139456,-0.131487321212171,
4.40473555835468));
#29002=CARTESIAN_POINT('Ctrl Pts',(4.81116921306824,-0.287199161490599,
4.32482210305491));
#29003=CARTESIAN_POINT('Ctrl Pts',(4.83502713109967,-0.407721671464292,
4.14749845969467));
#29004=CARTESIAN_POINT('Ctrl Pts',(4.85888504913109,-0.42854512664958,3.93410742516172));
#29005=CARTESIAN_POINT('Ctrl Pts',(4.8827429671625,-0.344577625034195,3.73682892005441));
#29006=CARTESIAN_POINT('Ctrl Pts',(4.90660088519393,-0.176351507991885,
3.60390291263011));
#29007=CARTESIAN_POINT('Ctrl Pts',(4.93045880322534,0.0349973564730633,
3.56783343253575));
#29008=CARTESIAN_POINT('Ctrl Pts',(4.95431672125677,0.237788413971502,3.63744045016736));
#29009=CARTESIAN_POINT('Ctrl Pts',(4.97817463928818,0.382433727027559,3.79570315365689));
#29010=CARTESIAN_POINT('Ctrl Pts',(5.0020325573196,0.433563576539811,4.00392200101168));
#29011=CARTESIAN_POINT('Ctrl Pts',(5.02589047535102,0.378675321553375,4.21118181228595));
#29012=CARTESIAN_POINT('Ctrl Pts',(5.04974839338244,0.231190635538481,4.36680191797922));
#29013=CARTESIAN_POINT('Ctrl Pts',(5.0666517869583,0.086644022961884,4.4135113916189));
#29014=CARTESIAN_POINT('Ctrl Pts',(5.07560254119034,0.00870023350343714,
4.41590490160082));
#29015=CARTESIAN_POINT('Ctrl Pts',(5.07660065607858,8.10857529294148E-6,
4.41589722116852));
#29016=CARTESIAN_POINT('Ctrl Pts',(4.8733993439214,-6.67049670157252E-6,
4.41584593494091));
#29017=CARTESIAN_POINT('Ctrl Pts',(4.87650074874903,-0.0270249643080214,
4.41586127519519));
#29018=CARTESIAN_POINT('Ctrl Pts',(4.88755479292047,-0.123313358466266,
4.40662010077424));
#29019=CARTESIAN_POINT('Ctrl Pts',(4.90656147643571,-0.277507970732168,
4.33313973520738));
#29020=CARTESIAN_POINT('Ctrl Pts',(4.93041939446713,-0.403200703213916,
4.15944262266324));
#29021=CARTESIAN_POINT('Ctrl Pts',(4.95427731249855,-0.430299880793222,
3.94675744574809));
#29022=CARTESIAN_POINT('Ctrl Pts',(4.97813523052996,-0.352179016385168,
3.7470915236456));
#29023=CARTESIAN_POINT('Ctrl Pts',(5.00199314856139,-0.187940789307144,
3.60926861310034));
#29024=CARTESIAN_POINT('Ctrl Pts',(5.0258510665928,0.0222540801607904,3.56699016996131));
#29025=CARTESIAN_POINT('Ctrl Pts',(5.04970898462423,0.227007220840439,3.63059442521772));
#29026=CARTESIAN_POINT('Ctrl Pts',(5.07356690265564,0.376250912472057,3.7845284059142));
#29027=CARTESIAN_POINT('Ctrl Pts',(5.09742482068706,0.433491007135177,3.99115106069306));
#29028=CARTESIAN_POINT('Ctrl Pts',(5.12128273871848,0.384730742495793,4.19993752217271));
#29029=CARTESIAN_POINT('Ctrl Pts',(5.1451406567499,0.241893331461176,4.35983381329239));
#29030=CARTESIAN_POINT('Ctrl Pts',(5.16251285848421,0.0948160588051851,
4.41219316122439));
#29031=CARTESIAN_POINT('Ctrl Pts',(5.17193242087471,0.0127860645481494,
4.41589818594594));
#29032=CARTESIAN_POINT('Ctrl Pts',(5.1733993439214,1.02299162792474E-5,
4.4158851107878));
#29033=CARTESIAN_POINT('Origin',(3.42660065607856,0.,4.));
#29034=CARTESIAN_POINT('',(4.47660065607858,-1.72413508574122E-6,4.41591032029986));
#29035=CARTESIAN_POINT('',(4.5733993439214,2.6062779713001E-6,4.4159095790646));
#29036=CARTESIAN_POINT('',(3.42660065607856,4.87367679877478E-13,4.415875));
#29037=CARTESIAN_POINT('Ctrl Pts',(4.47660065607858,-1.72413508575881E-6,
4.41591032029986));
#29038=CARTESIAN_POINT('Ctrl Pts',(4.47678655759518,-0.00162050728124812,
4.41591069657345));
#29039=CARTESIAN_POINT('Ctrl Pts',(4.48492509845559,-0.0724886630755744,
4.4155056303295));
#29040=CARTESIAN_POINT('Ctrl Pts',(4.5010162786598,-0.212178818846594,4.37811758201071));
#29041=CARTESIAN_POINT('Ctrl Pts',(4.52487419669122,-0.367409789343613,
4.23022337776645));
#29042=CARTESIAN_POINT('Ctrl Pts',(4.54873211472264,-0.432799058467291,
4.02603328640456));
#29043=CARTESIAN_POINT('Ctrl Pts',(4.57259003275406,-0.392357168499796,
3.8154773474345));
#29044=CARTESIAN_POINT('Ctrl Pts',(4.59644795078547,-0.255973263285106,
3.65004222328625));
#29045=CARTESIAN_POINT('Ctrl Pts',(4.6203058688169,-0.0569969226013119,
3.57018130821703));
#29046=CARTESIAN_POINT('Ctrl Pts',(4.64416378684831,0.155916718210686,3.59542277130738));
#29047=CARTESIAN_POINT('Ctrl Pts',(4.66802170487973,0.330704474340828,3.71959438727947));
#29048=CARTESIAN_POINT('Ctrl Pts',(4.69187962291115,0.424625978282027,3.91233281365517));
#29049=CARTESIAN_POINT('Ctrl Pts',(4.71573754094257,0.41471486395576,4.1265082550995));
#29050=CARTESIAN_POINT('Ctrl Pts',(4.73959545897399,0.303394668785218,4.30974898215573));
#29051=CARTESIAN_POINT('Ctrl Pts',(4.75988316401932,0.145646585585232,4.40116103141851));
#29052=CARTESIAN_POINT('Ctrl Pts',(4.77221822972086,0.0381762104768988,
4.41583012037823));
#29053=CARTESIAN_POINT('Ctrl Pts',(4.77660065607858,-3.27394476113199E-6,
4.41584059078717));
#29054=CARTESIAN_POINT('Ctrl Pts',(4.5733993439214,2.60627797130011E-6,
4.4159095790646));
#29055=CARTESIAN_POINT('Ctrl Pts',(4.58106907662335,-0.0667838229435618,
4.4158868274511));
#29056=CARTESIAN_POINT('Ctrl Pts',(4.59669144866912,-0.202842099803805,
4.38250385602613));
#29057=CARTESIAN_POINT('Ctrl Pts',(4.62026646005868,-0.360469908510665,
4.24094439618412));
#29058=CARTESIAN_POINT('Ctrl Pts',(4.6441243780901,-0.431844582779732,4.03876871570463));
#29059=CARTESIAN_POINT('Ctrl Pts',(4.66798229612152,-0.397621493350665,
3.82711302819544));
#29060=CARTESIAN_POINT('Ctrl Pts',(4.69184021415294,-0.266169117804412,
3.65773291463971));
#29061=CARTESIAN_POINT('Ctrl Pts',(4.71569813218436,-0.0696311426542753,
3.57204642662242));
#29062=CARTESIAN_POINT('Ctrl Pts',(4.73955605021577,0.143933543589337,3.59100624451743));
#29063=CARTESIAN_POINT('Ctrl Pts',(4.76341396824719,0.322302557754209,3.70997617639404));
#29064=CARTESIAN_POINT('Ctrl Pts',(4.78727188627862,0.421859817202848,3.8998648332327));
#29065=CARTESIAN_POINT('Ctrl Pts',(4.81112980431003,0.41826086011465,4.11423926597311));
#29066=CARTESIAN_POINT('Ctrl Pts',(4.83498772234146,0.312385729531365,4.30067908636799));
#29067=CARTESIAN_POINT('Ctrl Pts',(4.85574423554524,0.15381688120809,4.39891624198015));
#29068=CARTESIAN_POINT('Ctrl Pts',(4.86854810940522,0.04225549351942,4.41582193963064));
#29069=CARTESIAN_POINT('Ctrl Pts',(4.8733993439214,-6.67049670157252E-6,
4.41584593494091));
#29070=CARTESIAN_POINT('Origin',(3.42660065607856,0.,4.));
#29071=CARTESIAN_POINT('',(4.17660065607858,5.88453344125852E-6,4.41584444980552));
#29072=CARTESIAN_POINT('',(4.2733993439214,2.51014653358805E-6,4.41583996132385));
#29073=CARTESIAN_POINT('',(3.42660065607856,4.87367679877478E-13,4.415875));
#29074=CARTESIAN_POINT('Ctrl Pts',(4.17660065607858,5.88453344126799E-6,
4.41584444980552));
#29075=CARTESIAN_POINT('Ctrl Pts',(4.18135488546951,-0.0414115481342504,
4.41582334930757));
#29076=CARTESIAN_POINT('Ctrl Pts',(4.19406175420423,-0.152126265423154,
4.3993918905015));
#29077=CARTESIAN_POINT('Ctrl Pts',(4.21472126228278,-0.310547447266788,
4.30257739619942));
#29078=CARTESIAN_POINT('Ctrl Pts',(4.23857918031418,-0.417556725585918,
4.11678647978038));
#29079=CARTESIAN_POINT('Ctrl Pts',(4.26243709834561,-0.422462345057068,
3.90243789311793));
#29080=CARTESIAN_POINT('Ctrl Pts',(4.28629501637703,-0.324064236326554,
3.71194600226016));
#29081=CARTESIAN_POINT('Ctrl Pts',(4.31015293440845,-0.146423688323203,
3.59189110566319));
#29082=CARTESIAN_POINT('Ctrl Pts',(4.33401085243986,0.0670214896752265,
3.5716299793216));
#29083=CARTESIAN_POINT('Ctrl Pts',(4.35786877047129,0.264078061498623,3.65611697628114));
#29084=CARTESIAN_POINT('Ctrl Pts',(4.38172668850271,0.396560367883193,3.82469274783887));
#29085=CARTESIAN_POINT('Ctrl Pts',(4.40558460653412,0.432072854850341,4.03613591352675));
#29086=CARTESIAN_POINT('Ctrl Pts',(4.42944252456555,0.361931763288092,4.23874286631049));
#29087=CARTESIAN_POINT('Ctrl Pts',(4.45311454108036,0.204524647174786,4.38184685695289));
#29088=CARTESIAN_POINT('Ctrl Pts',(4.46883391825138,0.0676290543833733,
4.4158946000499));
#29089=CARTESIAN_POINT('Ctrl Pts',(4.47660065607858,-1.72413508575881E-6,
4.41591032029986));
#29090=CARTESIAN_POINT('Ctrl Pts',(4.2733993439214,2.51014653359152E-6,
4.41583996132385));
#29091=CARTESIAN_POINT('Ctrl Pts',(4.27768476515387,-0.0373320337329404,
4.41583213221101));
#29092=CARTESIAN_POINT('Ctrl Pts',(4.28992282573015,-0.143955736965383,
4.40160880992953));
#29093=CARTESIAN_POINT('Ctrl Pts',(4.31011352565024,-0.301501118270308,
4.3115924136571));
#29094=CARTESIAN_POINT('Ctrl Pts',(4.33397144368164,-0.413936097932681,
4.12903358037428));
#29095=CARTESIAN_POINT('Ctrl Pts',(4.35782936171308,-0.425152419412173,
3.91492252699502));
#29096=CARTESIAN_POINT('Ctrl Pts',(4.38168727974448,-0.332407397051365,
3.72161523052345));
#29097=CARTESIAN_POINT('Ctrl Pts',(4.40554519777592,-0.158379709595794,
3.5963805946708));
#29098=CARTESIAN_POINT('Ctrl Pts',(4.42940311580732,0.0543761300157755,
3.56984189703405));
#29099=CARTESIAN_POINT('Ctrl Pts',(4.45326103383876,0.25383552520097,3.64848857324589));
#29100=CARTESIAN_POINT('Ctrl Pts',(4.47711895187016,0.39122521984844,3.81308936806525));
#29101=CARTESIAN_POINT('Ctrl Pts',(4.50097686990159,0.432949691632991,4.02339490384879));
#29102=CARTESIAN_POINT('Ctrl Pts',(4.524834787933,0.368806170420464,4.22797974831721));
#29103=CARTESIAN_POINT('Ctrl Pts',(4.54869270596443,0.214479494504121,4.37681733431002));
#29104=CARTESIAN_POINT('Ctrl Pts',(4.56488089129389,0.0741790848482271,
4.4152866170047));
#29105=CARTESIAN_POINT('Ctrl Pts',(4.57311643727954,0.0024660981813593,
4.41591041828323));
#29106=CARTESIAN_POINT('Ctrl Pts',(4.5733993439214,2.60627797130011E-6,
4.4159095790646));
#29107=CARTESIAN_POINT('Origin',(4.,0.,4.));
#29108=CARTESIAN_POINT('',(4.,-7.34788079488412E-17,4.6));
#29109=CARTESIAN_POINT('Origin',(4.,0.,4.));
#29110=CARTESIAN_POINT('',(4.,-0.219892372742957,4.3529863453938));
#29111=CARTESIAN_POINT('Ctrl Pts',(4.,-0.219914231356238,4.35301468169996));
#29112=CARTESIAN_POINT('Ctrl Pts',(4.,-0.219843051329574,4.3531167999744));
#29113=CARTESIAN_POINT('Ctrl Pts',(4.,-0.219771822781512,4.35321888245988));
#29114=CARTESIAN_POINT('Ctrl Pts',(4.,-0.21970054575756,4.3533209291203));
#29115=CARTESIAN_POINT('Ctrl Pts',(4.,-0.207925336055227,4.3701793886806));
#29116=CARTESIAN_POINT('Ctrl Pts',(4.,-0.194831304039315,4.38605734350833));
#29117=CARTESIAN_POINT('Ctrl Pts',(4.,-0.18064579384139,4.40088380688851));
#29118=CARTESIAN_POINT('Ctrl Pts',(4.,-0.168975273508986,4.41308164397169));
#29119=CARTESIAN_POINT('Ctrl Pts',(4.,-0.156565051628872,4.42456888924957));
#29120=CARTESIAN_POINT('Ctrl Pts',(4.,-0.143515931303371,4.43531683418355));
#29121=CARTESIAN_POINT('Ctrl Pts',(4.,-0.133182439541062,4.44382804395605));
#29122=CARTESIAN_POINT('Ctrl Pts',(4.,-0.122447811630206,4.45187590303098));
#29123=CARTESIAN_POINT('Ctrl Pts',(4.,-0.111352162047151,4.45944712768208));
#29124=CARTESIAN_POINT('Ctrl Pts',(4.,-0.105068105051177,4.46373511522897));
#29125=CARTESIAN_POINT('Ctrl Pts',(4.,-0.0986661212125077,4.46787107983396));
#29126=CARTESIAN_POINT('Ctrl Pts',(4.,-0.0921733602714696,4.47184061613108));
#29127=CARTESIAN_POINT('Ctrl Pts',(4.,-0.0718171345235072,4.48428598070136));
#29128=CARTESIAN_POINT('Ctrl Pts',(4.,-0.0505350523745213,4.49512244469223));
#29129=CARTESIAN_POINT('Ctrl Pts',(4.,-0.0285775088988711,4.50429938857761));
#29130=CARTESIAN_POINT('Ctrl Pts',(4.,-0.00645956782426854,4.51354336909515));
#29131=CARTESIAN_POINT('Ctrl Pts',(4.,0.0163444141029789,4.52110543571878));
#29132=CARTESIAN_POINT('Ctrl Pts',(4.,0.0396343143342583,4.52702898180467));
#29133=CARTESIAN_POINT('Ctrl Pts',(4.,0.0479455316904685,4.52914285427945));
#29134=CARTESIAN_POINT('Ctrl Pts',(4.,0.0563191235587283,4.53104786585874));
#29135=CARTESIAN_POINT('Ctrl Pts',(4.,0.0647475081636451,4.53274519105122));
#29136=CARTESIAN_POINT('Ctrl Pts',(4.,0.0709442475001029,4.53399310299165));
#29137=CARTESIAN_POINT('Ctrl Pts',(4.,0.0771669940275102,4.53512789739638));
#29138=CARTESIAN_POINT('Ctrl Pts',(4.,0.0834037601527001,4.53614909266968));
#29139=CARTESIAN_POINT('Ctrl Pts',(4.,0.108500755516298,4.54025842313435));
#29140=CARTESIAN_POINT('Ctrl Pts',(4.,0.133859781029961,4.54253781872753));
#29141=CARTESIAN_POINT('Ctrl Pts',(3.99999999999999,0.159256593756596,4.54305292380224));
#29142=CARTESIAN_POINT('Ctrl Pts',(3.99999999999999,0.185497795908202,4.5435851550133));
#29143=CARTESIAN_POINT('Ctrl Pts',(3.99999999999998,0.211780221987087,4.54223483664603));
#29144=CARTESIAN_POINT('Ctrl Pts',(3.99999999999998,0.237902321580844,4.5390442708621));
#29145=CARTESIAN_POINT('Ctrl Pts',(3.99999999999998,0.243507595489062,4.53835964001621));
#29146=CARTESIAN_POINT('Ctrl Pts',(3.99999999999998,0.249105619801251,4.53759013757336));
#29147=CARTESIAN_POINT('Ctrl Pts',(3.99999999999998,0.254694598474614,4.53673594206822));
#29148=CARTESIAN_POINT('',(4.,-0.219892372743086,3.64701365460628));
#29149=CARTESIAN_POINT('Ctrl Pts',(4.,0.254721014554616,3.46322028700966));
#29150=CARTESIAN_POINT('Ctrl Pts',(4.,0.254552373521139,3.46319452321125));
#29151=CARTESIAN_POINT('Ctrl Pts',(4.,0.254383724765285,3.46316883668624));
#29152=CARTESIAN_POINT('Ctrl Pts',(4.,0.254215068323085,3.46314322746093));
#29153=CARTESIAN_POINT('Ctrl Pts',(4.,0.228435861761457,3.4592288468388));
#29154=CARTESIAN_POINT('Ctrl Pts',(4.,0.202474691352968,3.45711700011808));
#29155=CARTESIAN_POINT('Ctrl Pts',(4.,0.176517231963435,3.45683380906617));
#29156=CARTESIAN_POINT('Ctrl Pts',(4.,0.151199179447316,3.45655759382427));
#29157=CARTESIAN_POINT('Ctrl Pts',(4.,0.125883695414598,3.45802192769867));
#29158=CARTESIAN_POINT('Ctrl Pts',(4.,0.1007794950383,3.46128259448669));
#29159=CARTESIAN_POINT('Ctrl Pts',(4.,0.0854593772715275,3.46327245269535));
#29160=CARTESIAN_POINT('Ctrl Pts',(4.,0.0702187270328167,3.46593187194604));
#29161=CARTESIAN_POINT('Ctrl Pts',(4.,0.0551140352340102,3.4692772918897));
#29162=CARTESIAN_POINT('Ctrl Pts',(4.,0.0468842919617017,3.47110003330284));
#29163=CARTESIAN_POINT('Ctrl Pts',(4.,0.0386923719445779,3.47312744960567));
#29164=CARTESIAN_POINT('Ctrl Pts',(4.,0.0305707631998946,3.47535548770785));
#29165=CARTESIAN_POINT('Ctrl Pts',(4.,0.0102648423897012,3.48092610391051));
#29166=CARTESIAN_POINT('Ctrl Pts',(4.,-0.00963556638195036,3.48775588581666));
#29167=CARTESIAN_POINT('Ctrl Pts',(4.,-0.0289965775380143,3.49587186612014));
#29168=CARTESIAN_POINT('Ctrl Pts',(4.,-0.047965755796229,3.50382359322137));
#29169=CARTESIAN_POINT('Ctrl Pts',(4.,-0.0664174073931304,3.51301096346156));
#29170=CARTESIAN_POINT('Ctrl Pts',(4.,-0.0841982143338667,3.52340033683134));
#29171=CARTESIAN_POINT('Ctrl Pts',(4.,-0.0930898199841631,3.5285957259532));
#29172=CARTESIAN_POINT('Ctrl Pts',(4.,-0.101813128894432,3.53409169793663));
#29173=CARTESIAN_POINT('Ctrl Pts',(4.,-0.110345561972859,3.53988353361915));
#29174=CARTESIAN_POINT('Ctrl Pts',(4.,-0.11586100642067,3.5436274303089));
#29175=CARTESIAN_POINT('Ctrl Pts',(4.,-0.121288652521606,3.54748953413154));
#29176=CARTESIAN_POINT('Ctrl Pts',(4.,-0.126621987542688,3.55146681430013));
#29177=CARTESIAN_POINT('Ctrl Pts',(4.,-0.143297831161627,3.56390265451229));
#29178=CARTESIAN_POINT('Ctrl Pts',(4.,-0.159061930875806,3.57746928852925));
#29179=CARTESIAN_POINT('Ctrl Pts',(4.,-0.173743808224101,3.59211536896244));
#29180=CARTESIAN_POINT('Ctrl Pts',(4.,-0.187864697165731,3.60620182877415));
#29181=CARTESIAN_POINT('Ctrl Pts',(4.,-0.200984288190684,3.62128798311348));
#29182=CARTESIAN_POINT('Ctrl Pts',(4.,-0.212904831975564,3.63731335989365));
#29183=CARTESIAN_POINT('Ctrl Pts',(4.,-0.21528245268753,3.64050971304978));
#29184=CARTESIAN_POINT('Ctrl Pts',(4.,-0.217612227418936,3.64374335030505));
#29185=CARTESIAN_POINT('Ctrl Pts',(4.,-0.219892372743211,3.64701365460636));
#29186=CARTESIAN_POINT('Origin',(4.,0.,4.));
#29187=CARTESIAN_POINT('Origin',(2.,0.,4.));
#29188=CARTESIAN_POINT('',(2.,-7.34788079488412E-17,4.6));
#29189=CARTESIAN_POINT('',(2.,-7.34788079488412E-17,4.6));
#29190=CARTESIAN_POINT('Origin',(2.,0.,4.));
#29191=CARTESIAN_POINT('Origin',(2.,0.,4.));
#29192=CARTESIAN_POINT('Ctrl Pts',(3.95224475517895,0.178288362465424,4.37571967666652));
#29193=CARTESIAN_POINT('Ctrl Pts',(3.96019739452275,0.115708609995841,4.40541533085819));
#29194=CARTESIAN_POINT('Ctrl Pts',(3.97610267321037,-0.0245105356436035,
4.43290545314371));
#29195=CARTESIAN_POINT('Ctrl Pts',(3.99996059124178,-0.228962993402626,
4.36819499612132));
#29196=CARTESIAN_POINT('Ctrl Pts',(4.0238185092732,-0.377374743411151,4.21349068386271));
#29197=CARTESIAN_POINT('Ctrl Pts',(4.04767642730463,-0.433534992178268,
4.00656196868444));
#29198=CARTESIAN_POINT('Ctrl Pts',(4.07153434533603,-0.383670022685343,
3.79803920418254));
#29199=CARTESIAN_POINT('Ctrl Pts',(4.09539226336747,-0.239994733226421,
3.63889579340969));
#29200=CARTESIAN_POINT('Ctrl Pts',(4.11925018139887,-0.0376302499649443,
3.56805514133307));
#29201=CARTESIAN_POINT('Ctrl Pts',(4.1431080994303,0.173933765839147,3.60283521426327));
#29202=CARTESIAN_POINT('Ctrl Pts',(4.16696601746172,0.342967344134064,3.73473372141871));
#29203=CARTESIAN_POINT('Ctrl Pts',(4.19082393549313,0.428135478754777,3.93149662217858));
#29204=CARTESIAN_POINT('Ctrl Pts',(4.21468185352456,0.40861313688017,4.1450106963618));
#29205=CARTESIAN_POINT('Ctrl Pts',(4.23853977155597,0.289173588337559,4.32306558264197));
#29206=CARTESIAN_POINT('Ctrl Pts',(4.2623976895874,0.0990233075312312,4.42212219878201));
#29207=CARTESIAN_POINT('Ctrl Pts',(4.28625560761881,-0.115340915390822,
4.41795840454656));
#29208=CARTESIAN_POINT('Ctrl Pts',(4.31011352565024,-0.301501118270308,
4.3115924136571));
#29209=CARTESIAN_POINT('Ctrl Pts',(4.33397144368164,-0.413936097932681,
4.12903358037428));
#29210=CARTESIAN_POINT('Ctrl Pts',(4.35782936171308,-0.425152419412173,
3.91492252699502));
#29211=CARTESIAN_POINT('Ctrl Pts',(4.38168727974448,-0.332407397051365,
3.72161523052345));
#29212=CARTESIAN_POINT('Ctrl Pts',(4.40554519777592,-0.158379709595794,
3.5963805946708));
#29213=CARTESIAN_POINT('Ctrl Pts',(4.42940311580732,0.0543761300157755,
3.56984189703405));
#29214=CARTESIAN_POINT('Ctrl Pts',(4.45326103383876,0.25383552520097,3.64848857324589));
#29215=CARTESIAN_POINT('Ctrl Pts',(4.47711895187016,0.39122521984844,3.81308936806525));
#29216=CARTESIAN_POINT('Ctrl Pts',(4.50097686990159,0.432949691632991,4.02339490384879));
#29217=CARTESIAN_POINT('Ctrl Pts',(4.524834787933,0.368806170420464,4.22797974831721));
#29218=CARTESIAN_POINT('Ctrl Pts',(4.54869270596443,0.214479494504121,4.37681733431002));
#29219=CARTESIAN_POINT('Ctrl Pts',(4.57255062399584,0.00770673985495463,
4.4335128177492));
#29220=CARTESIAN_POINT('Ctrl Pts',(4.59640854202726,-0.200950522604244,
4.38420260860549));
#29221=CARTESIAN_POINT('Ctrl Pts',(4.62026646005868,-0.360469908510665,
4.24094439618412));
#29222=CARTESIAN_POINT('Ctrl Pts',(4.6441243780901,-0.431844582779732,4.03876871570463));
#29223=CARTESIAN_POINT('Ctrl Pts',(4.66798229612152,-0.397621493350665,
3.82711302819544));
#29224=CARTESIAN_POINT('Ctrl Pts',(4.69184021415294,-0.266169117804412,
3.65773291463971));
#29225=CARTESIAN_POINT('Ctrl Pts',(4.71569813218436,-0.0696311426542753,
3.57204642662242));
#29226=CARTESIAN_POINT('Ctrl Pts',(4.73955605021577,0.143933543589337,3.59100624451743));
#29227=CARTESIAN_POINT('Ctrl Pts',(4.76341396824719,0.322302557754209,3.70997617639404));
#29228=CARTESIAN_POINT('Ctrl Pts',(4.78727188627862,0.421859817202848,3.8998648332327));
#29229=CARTESIAN_POINT('Ctrl Pts',(4.81112980431003,0.41826086011465,4.11423926597311));
#29230=CARTESIAN_POINT('Ctrl Pts',(4.83498772234146,0.312385729531365,4.30067908636799));
#29231=CARTESIAN_POINT('Ctrl Pts',(4.85884564037287,0.130123778861223,4.41359467981201));
#29232=CARTESIAN_POINT('Ctrl Pts',(4.88270355840429,-0.0839569802410516,
4.42537510794913));
#29233=CARTESIAN_POINT('Ctrl Pts',(4.90656147643571,-0.277507970732168,
4.33313973520738));
#29234=CARTESIAN_POINT('Ctrl Pts',(4.93041939446713,-0.403200703213916,
4.15944262266324));
#29235=CARTESIAN_POINT('Ctrl Pts',(4.95427731249855,-0.430299880793222,
3.94675744574809));
#29236=CARTESIAN_POINT('Ctrl Pts',(4.97813523052996,-0.352179016385168,
3.7470915236456));
#29237=CARTESIAN_POINT('Ctrl Pts',(5.00199314856139,-0.187940789307144,
3.60926861310034));
#29238=CARTESIAN_POINT('Ctrl Pts',(5.0258510665928,0.0222540801607904,3.56699016996131));
#29239=CARTESIAN_POINT('Ctrl Pts',(5.04970898462423,0.227007220840439,3.63059442521772));
#29240=CARTESIAN_POINT('Ctrl Pts',(5.07356690265564,0.376250912472057,3.7845284059142));
#29241=CARTESIAN_POINT('Ctrl Pts',(5.09742482068706,0.433491007135177,3.99115106069306));
#29242=CARTESIAN_POINT('Ctrl Pts',(5.12128273871848,0.384730742495793,4.19993752217271));
#29243=CARTESIAN_POINT('Ctrl Pts',(5.1451406567499,0.241893331461176,4.35983381329239));
#29244=CARTESIAN_POINT('Ctrl Pts',(5.16899857478132,0.0399064118422473,
4.43174093538579));
#29245=CARTESIAN_POINT('Ctrl Pts',(5.19285649281273,-0.171838712500945,
4.39807563839043));
#29246=CARTESIAN_POINT('Ctrl Pts',(5.21671441084416,-0.341564590845109,
4.26707000444592));
#29247=CARTESIAN_POINT('Ctrl Pts',(5.24057232887557,-0.427768622694993,
4.07075847957352));
#29248=CARTESIAN_POINT('Ctrl Pts',(5.264430246907,-0.409371574112622,3.85714457902312));
#29249=CARTESIAN_POINT('Ctrl Pts',(5.2882881649384,-0.290872024601924,3.6784627202051));
#29250=CARTESIAN_POINT('Ctrl Pts',(5.31214608296984,-0.101246341881189,
3.57840548479658));
#29251=CARTESIAN_POINT('Ctrl Pts',(5.33600400100125,0.113136829324483,3.58143959235932));
#29252=CARTESIAN_POINT('Ctrl Pts',(5.35986191903268,0.299854963974951,3.68682312094679));
#29253=CARTESIAN_POINT('Ctrl Pts',(5.38371983706408,0.413250392048343,3.8687869272297));
#29254=CARTESIAN_POINT('Ctrl Pts',(5.40757775509551,0.425594842551202,4.08283590397723));
#29255=CARTESIAN_POINT('Ctrl Pts',(5.43143567312693,0.333869761079625,4.27662924579771));
#29256=CARTESIAN_POINT('Ctrl Pts',(5.45529359115834,0.160504428594232,4.4027792017911));
#29257=CARTESIAN_POINT('Ctrl Pts',(5.47915150918977,-0.0521086087350157,
4.43043867146175));
#29258=CARTESIAN_POINT('Ctrl Pts',(5.50300942722118,-0.251979671819092,
4.35284416104532));
#29259=CARTESIAN_POINT('Ctrl Pts',(5.52686734525261,-0.390234841353927,
4.18896964197264));
#29260=CARTESIAN_POINT('Ctrl Pts',(5.55072526328402,-0.433066962396004,
3.97888689800548));
#29261=CARTESIAN_POINT('Ctrl Pts',(5.57458318131544,-0.370002414621403,
3.77396688259));
#29262=CARTESIAN_POINT('Ctrl Pts',(5.59844109934686,-0.21646219781534,3.62431812139094));
#29263=CARTESIAN_POINT('Ctrl Pts',(5.62229901737828,-0.00999107731853999,
3.56653381289738));
#29264=CARTESIAN_POINT('Ctrl Pts',(5.64615693540971,0.198923133709572,3.61474379450078));
#29265=CARTESIAN_POINT('Ctrl Pts',(5.67001485344111,0.359195220034686,3.75715941257656));
#29266=CARTESIAN_POINT('Ctrl Pts',(5.69387277147254,0.431634290692432,3.95895616900985));
#29267=CARTESIAN_POINT('Ctrl Pts',(5.71773068950395,0.398527019959163,4.1707892603438));
#29268=CARTESIAN_POINT('Ctrl Pts',(5.74158860753538,0.267969036875697,4.34085972491723));
#29269=CARTESIAN_POINT('Ctrl Pts',(5.76544652556679,0.0718853255354575,
4.42758070267197));
#29270=CARTESIAN_POINT('Ctrl Pts',(5.78930444359821,-0.141776307127955,
4.40974655013133));
#29271=CARTESIAN_POINT('Ctrl Pts',(5.81316236162963,-0.320769768688322,
4.29171820750724));
#29272=CARTESIAN_POINT('Ctrl Pts',(5.83702027966105,-0.421326288178809,
4.10235681181338));
#29273=CARTESIAN_POINT('Ctrl Pts',(5.86087819769247,-0.418857046020503,
3.88796639709818));
#29274=CARTESIAN_POINT('Ctrl Pts',(5.88473611572389,-0.313965860818636,
3.70097123187977));
#29275=CARTESIAN_POINT('Ctrl Pts',(5.90859403375531,-0.132301443679057,
3.58709678011166));
#29276=CARTESIAN_POINT('Ctrl Pts',(5.93245195178673,0.0817142298265842,
3.57418834816524));
#29277=CARTESIAN_POINT('Ctrl Pts',(5.95630986981814,0.275748643515392,3.66540258613358));
#29278=CARTESIAN_POINT('Ctrl Pts',(5.98016778784957,0.402354822815078,3.83843477537114));
#29279=CARTESIAN_POINT('Ctrl Pts',(6.00402570588098,0.430574627524036,4.05097449853386));
#29280=CARTESIAN_POINT('Ctrl Pts',(6.02788362391241,0.353506566116634,4.25104874587108));
#29281=CARTESIAN_POINT('Ctrl Pts',(6.05174154194382,0.189997730437525,4.38973628930191));
#29282=CARTESIAN_POINT('Ctrl Pts',(6.07559945997525,-0.0199730113800777,
4.43311976162365));
#29283=CARTESIAN_POINT('Ctrl Pts',(6.09945737800665,-0.2250554921608,4.3705991908187));
#29284=CARTESIAN_POINT('Ctrl Pts',(6.12331529603809,-0.375113923638194,
4.21744656883549));
#29285=CARTESIAN_POINT('Ctrl Pts',(6.1471732140695,-0.433431396087355,4.01114207710762));
#29286=CARTESIAN_POINT('Ctrl Pts',(6.17103113210093,-0.385792139046387,
3.80207577201042));
#29287=CARTESIAN_POINT('Ctrl Pts',(6.19488905013233,-0.243761337718234,
3.64147770828707));
#29288=CARTESIAN_POINT('Ctrl Pts',(6.21874696816376,-0.042227823444436,
3.56841523311022));
#29289=CARTESIAN_POINT('Ctrl Pts',(6.24260488619517,0.16982704650124,3.60113783246665));
#29290=CARTESIAN_POINT('Ctrl Pts',(6.2664628042266,0.339985970990829,3.73091992247201));
#29291=CARTESIAN_POINT('Ctrl Pts',(6.29032072225801,0.427700638223926,3.92738904240251));
#29292=CARTESIAN_POINT('Ctrl Pts',(6.31417864028943,0.409561128158778,4.13996490148311));
#29293=CARTESIAN_POINT('Ctrl Pts',(6.34598919766466,0.254661277208374,4.38159318714805));
#29294=CARTESIAN_POINT('Ctrl Pts',(6.38575239438369,-0.125272905304917,
4.47558432627151));
#29295=CARTESIAN_POINT('Ctrl Pts',(6.43346823044653,-0.468271923807345,
4.15124960425567));
#29296=CARTESIAN_POINT('Ctrl Pts',(6.48118406650937,-0.380227249479543,
3.6882349865083));
#29297=CARTESIAN_POINT('Ctrl Pts',(6.52889990257221,0.0564566449812287,
3.51140415777354));
#29298=CARTESIAN_POINT('Ctrl Pts',(6.57661573863504,0.441574375138847,3.78331933667001));
#29299=CARTESIAN_POINT('Ctrl Pts',(6.62433157469789,0.421040068198854,4.25418342072721));
#29300=CARTESIAN_POINT('Ctrl Pts',(6.67204741076071,0.0139362792425842,
4.49164405688148));
#29301=CARTESIAN_POINT('Ctrl Pts',(6.71976324682356,-0.406006764042365,
4.27761133505345));
#29302=CARTESIAN_POINT('Ctrl Pts',(6.76747908288639,-0.453085647428837,
3.80864864857145));
#29303=CARTESIAN_POINT('Ctrl Pts',(6.81519491894923,-0.0841006081168706,
3.51540431248109));
#29304=CARTESIAN_POINT('Ctrl Pts',(6.86291075501207,0.362121456530253,3.66717299786736));
#29305=CARTESIAN_POINT('Ctrl Pts',(6.91062659107491,0.475798562415156,4.124581128109));
#29306=CARTESIAN_POINT('Ctrl Pts',(6.95834242713775,0.152544250279933,4.46758486877347));
#29307=CARTESIAN_POINT('Ctrl Pts',(7.00605826320058,-0.310794706562241,
4.38119802990972));
#29308=CARTESIAN_POINT('Ctrl Pts',(7.05377409926342,-0.488725618924084,
3.94475128051735));
#29309=CARTESIAN_POINT('Ctrl Pts',(7.10148993532626,-0.21785253135038,3.55904022429238));
#29310=CARTESIAN_POINT('Ctrl Pts',(7.14920577138909,0.253078023397415,3.57826934481931));
#29311=CARTESIAN_POINT('Ctrl Pts',(7.19692160745195,0.491603063369337,3.98478019943955));
#29312=CARTESIAN_POINT('Ctrl Pts',(7.24463744351477,0.278681483980911,4.40526763942622));
#29313=CARTESIAN_POINT('Ctrl Pts',(7.29235327957762,-0.190157610347023,
4.45359156587464));
#29314=CARTESIAN_POINT('Ctrl Pts',(7.34006911564044,-0.484372034479295,
4.08537538031203));
#29315=CARTESIAN_POINT('Ctrl Pts',(7.3877849517033,-0.333780171974684,3.63875766810317));
#29316=CARTESIAN_POINT('Ctrl Pts',(7.43550078776612,0.123327161313159,3.52387434835784));
#29317=CARTESIAN_POINT('Ctrl Pts',(7.48321662382897,0.467181263150904,3.84622454030349));
#29318=CARTESIAN_POINT('Ctrl Pts',(7.5309324598918,0.382015623368301,4.30978910321172));
#29319=CARTESIAN_POINT('Ctrl Pts',(7.57864829595465,-0.0539608418635878,
4.4888695658253));
#29320=CARTESIAN_POINT('Ctrl Pts',(7.62636413201748,-0.440384235482588,
4.21901358396786));
#29321=CARTESIAN_POINT('Ctrl Pts',(7.67407996808031,-0.422396009600076,
3.7480340579683));
#29322=CARTESIAN_POINT('Ctrl Pts',(7.72179580414317,-0.0165150286377962,
3.50843873354525));
#29323=CARTESIAN_POINT('Ctrl Pts',(7.76951164020598,0.404531957204003,3.72025168374225));
#29324=CARTESIAN_POINT('Ctrl Pts',(7.81722747626884,0.454091022239626,4.18896181724392));
#29325=CARTESIAN_POINT('Ctrl Pts',(7.86494331233166,0.0866513144543145,
4.48414540641706));
#29326=CARTESIAN_POINT('Ctrl Pts',(7.91265914839452,-0.360361628691054,
4.33473081934393));
#29327=CARTESIAN_POINT('Ctrl Pts',(7.96037498445733,-0.476448943335793,
3.87792777037096));
#29328=CARTESIAN_POINT('Ctrl Pts',(8.0080908205202,-0.1550058622045,3.53322552818936));
#29329=CARTESIAN_POINT('Ctrl Pts',(8.05580665658301,0.308781487260178,3.61716946571973));
#29330=CARTESIAN_POINT('Ctrl Pts',(8.10352249264587,0.489010045760349,4.0526725734847));
#29331=CARTESIAN_POINT('Ctrl Pts',(8.1512383287087,0.220173154851853,4.43980564654689));
#29332=CARTESIAN_POINT('Ctrl Pts',(8.19895416477154,-0.250852131956433,
4.4230584271054));
#29333=CARTESIAN_POINT('Ctrl Pts',(8.24667000083438,-0.491516046133,4.01781014446235));
#29334=CARTESIAN_POINT('Ctrl Pts',(8.29438583689722,-0.280813212199106,
3.59620653211525));
#29335=CARTESIAN_POINT('Ctrl Pts',(8.34210167296004,0.187764715363875,3.54541267448783));
#29336=CARTESIAN_POINT('Ctrl Pts',(8.38981750902289,0.483915415676709,3.91207335260334));
#29337=CARTESIAN_POINT('Ctrl Pts',(8.43753334508573,0.335679143777854,4.35947842394856));
#29338=CARTESIAN_POINT('Ctrl Pts',(8.48524918114857,-0.120816450939738,
4.4767689272953));
#29339=CARTESIAN_POINT('Ctrl Pts',(8.5329650172114,-0.466364439759318,4.15623518867385));
#29340=CARTESIAN_POINT('Ctrl Pts',(8.58068085327425,-0.383642787608637,
3.69222827230584));
#29341=CARTESIAN_POINT('Ctrl Pts',(8.62839668933707,0.0513839395061145,
3.51085286915611));
#29342=CARTESIAN_POINT('Ctrl Pts',(8.67611252539993,0.439224004328866,3.77866880275638));
#29343=CARTESIAN_POINT('Ctrl Pts',(8.72382836146275,0.42371790764641,4.24973658040369));
#29344=CARTESIAN_POINT('Ctrl Pts',(8.7715441975256,0.0191051366342138,4.49146741357506));
#29345=CARTESIAN_POINT('Ctrl Pts',(8.81926003358843,-0.403052175319494,
4.28187615866228));
#29346=CARTESIAN_POINT('Ctrl Pts',(8.86697586965126,-0.455080472922433,
3.81343369002772));
#29347=CARTESIAN_POINT('Ctrl Pts',(8.91469170571412,-0.0892013699275644,
3.51631793453238));
#29348=CARTESIAN_POINT('Ctrl Pts',(8.96240754177693,0.358592723611288,3.66337486216116));
#29349=CARTESIAN_POINT('Ctrl Pts',(9.0101233778398,0.477085601399612,4.11955983351088));
#29350=CARTESIAN_POINT('Ctrl Pts',(9.05783921390261,0.157463430517111,4.46595117008304));
#29351=CARTESIAN_POINT('Ctrl Pts',(9.10555504996547,-0.306759831495564,
4.38445237758765));
#29352=CARTESIAN_POINT('Ctrl Pts',(9.1532708860283,-0.489280820139143,3.94990505119329));
#29353=CARTESIAN_POINT('Ctrl Pts',(9.20098672209113,-0.222487703095825,
3.56136068709803));
#29354=CARTESIAN_POINT('Ctrl Pts',(9.24870255815399,0.248619295113741,3.57562555337399));
#29355=CARTESIAN_POINT('Ctrl Pts',(9.29641839421681,0.49141536912078,3.97960000382683));
#29356=CARTESIAN_POINT('Ctrl Pts',(9.34413423027966,0.282937148266828,4.40230808465976));
#29357=CARTESIAN_POINT('Ctrl Pts',(9.39185006634249,-0.185366609388173,
4.45557046104408));
#29358=CARTESIAN_POINT('Ctrl Pts',(9.43956590240532,-0.483445357410111,
4.09047547319903));
#29359=CARTESIAN_POINT('Ctrl Pts',(9.48728173846818,-0.337568794959357,
3.64229546617122));
#29360=CARTESIAN_POINT('Ctrl Pts',(9.53499757453099,0.118302386066128,3.5226010365501));
#29361=CARTESIAN_POINT('Ctrl Pts',(9.58271341059386,0.465534665650901,3.84130942079228));
#29362=CARTESIAN_POINT('Ctrl Pts',(9.63042924665667,0.385259298596883,4.30574580568933));
#29363=CARTESIAN_POINT('Ctrl Pts',(9.67814508271952,-0.0488056103349303,
4.48941111271794));
#29364=CARTESIAN_POINT('Ctrl Pts',(9.72586091878235,-0.438051576325333,
4.22364266437974));
#29365=CARTESIAN_POINT('Ctrl Pts',(9.77357675484519,-0.425028039486299,
3.75249971615691));
#29366=CARTESIAN_POINT('Ctrl Pts',(9.82129259090803,-0.0216947140899849,
3.50864008686857));
#29367=CARTESIAN_POINT('Ctrl Pts',(9.86900842697087,0.401561201071248,3.7160038263529));
#29368=CARTESIAN_POINT('Ctrl Pts',(9.91672426303371,0.456057286475463,4.18416562194019));
#29369=CARTESIAN_POINT('Ctrl Pts',(9.96444009909655,0.0917489483659128,
4.48320529314746));
#29370=CARTESIAN_POINT('Ctrl Pts',(10.0121559351594,-0.356813860767086,
4.3385101085883));
#29371=CARTESIAN_POINT('Ctrl Pts',(10.0598717712222,-0.477709011270712,
3.88295588266498));
#29372=CARTESIAN_POINT('Ctrl Pts',(10.1075876072851,-0.159916626226494,
3.53488507064564));
#29373=CARTESIAN_POINT('Ctrl Pts',(10.1553034433479,0.304729657315094,3.61393645496551));
#29374=CARTESIAN_POINT('Ctrl Pts',(10.2030192794107,0.489538007675758,4.04751593304174));
#29375=CARTESIAN_POINT('Ctrl Pts',(10.2507351154736,0.224796073077312,4.43746079867915));
#29376=CARTESIAN_POINT('Ctrl Pts',(10.2984509515364,-0.246379554360218,
4.42567868168988));
#29377=CARTESIAN_POINT('Ctrl Pts',(10.3461667875993,-0.491301045992024,
4.02298928139638));
#29378=CARTESIAN_POINT('Ctrl Pts',(10.3938826236621,-0.285053227451061,
3.599188470261));
#29379=CARTESIAN_POINT('Ctrl Pts',(10.4415984597249,0.182963355965895,3.54345905416307));
#29380=CARTESIAN_POINT('Ctrl Pts',(10.4893142957878,0.482961874346273,3.9069782134126));
#29381=CARTESIAN_POINT('Ctrl Pts',(10.5370301318506,0.339449072190825,4.35592071060949));
#29382=CARTESIAN_POINT('Ctrl Pts',(10.5847459679134,-0.115785036052801,
4.47801574270962));
#29383=CARTESIAN_POINT('Ctrl Pts',(10.6324618039763,-0.464691964107356,
4.16114156306187));
#29384=CARTESIAN_POINT('Ctrl Pts',(10.6801776400391,-0.386865111317189,
3.69628860657276));
#29385=CARTESIAN_POINT('Ctrl Pts',(10.7278934761019,0.0462259258804368,
3.51033849586834));
#29386=CARTESIAN_POINT('Ctrl Pts',(10.7756093121648,0.436866984064762,3.77405207881873));
#29387=CARTESIAN_POINT('Ctrl Pts',(10.8233251482276,0.426326368719826,4.24525711444552));
#29388=CARTESIAN_POINT('Ctrl Pts',(10.8710409842905,0.0242836891050981,
4.49123876811122));
#29389=CARTESIAN_POINT('Ctrl Pts',(10.9187568203533,-0.400059075867425,
4.28610830234036));
#29390=CARTESIAN_POINT('Ctrl Pts',(10.9664726564161,-0.45702143577077,3.81824018018824));
#29391=CARTESIAN_POINT('Ctrl Pts',(11.014188492479,-0.0942939790271268,
3.51728489730359));
#29392=CARTESIAN_POINT('Ctrl Pts',(11.0619043285418,0.355025089556487,3.65961432075161));
#29393=CARTESIAN_POINT('Ctrl Pts',(11.1096201646047,0.478319155637209,4.11452515096033));
#29394=CARTESIAN_POINT('Ctrl Pts',(11.1573360006675,0.16236538121005,4.46426577284621));
#29395=CARTESIAN_POINT('Ctrl Pts',(11.2050518367304,-0.302691021094817,
4.38766399188028));
#29396=CARTESIAN_POINT('Ctrl Pts',(11.2527676727932,-0.489781601228288,
3.95506440219344));
#29397=CARTESIAN_POINT('Ctrl Pts',(11.300483508856,-0.227098200695192,3.56372986339542));
#29398=CARTESIAN_POINT('Ctrl Pts',(11.3481993449188,0.244132971891272,3.57302890392028));
#29399=CARTESIAN_POINT('Ctrl Pts',(11.3959151809817,0.491173079921361,3.97442207176994));
#29400=CARTESIAN_POINT('Ctrl Pts',(11.4436310170445,0.287161390990383,4.39930384468027));
#29401=CARTESIAN_POINT('Ctrl Pts',(11.4913468531074,-0.180555021833016,
4.45749875294131));
#29402=CARTESIAN_POINT('Ctrl Pts',(11.5390626891702,-0.482464979911041,
4.09556551685319));
#29403=CARTESIAN_POINT('Ctrl Pts',(11.586778525233,-0.341319923258817,3.64587299617429));
#29404=CARTESIAN_POINT('Ctrl Pts',(11.6344943612959,0.113264470804062,3.5213807520529));
#29405=CARTESIAN_POINT('Ctrl Pts',(11.6822101973587,0.463836358529674,3.83641192782507));
#29406=CARTESIAN_POINT('Ctrl Pts',(11.7299260334216,0.38846018117773,4.30166854740152));
#29407=CARTESIAN_POINT('Ctrl Pts',(11.7776418694844,-0.0436449577779122,
4.48989829813191));
#29408=CARTESIAN_POINT('Ctrl Pts',(11.8253577055472,-0.435670260442099,
4.22824690363353));
#29409=CARTESIAN_POINT('Ctrl Pts',(11.8730735416101,-0.427612859293677,
3.75699286549843));
#29410=CARTESIAN_POINT('Ctrl Pts',(11.9207893776729,-0.0268719897862959,
3.50889601812151));
#29411=CARTESIAN_POINT('Ctrl Pts',(11.9685052137357,0.398545841420554,3.71178751390968));
#29412=CARTESIAN_POINT('Ctrl Pts',(12.0162210497986,0.457972894034889,4.17934897039372));
#29413=CARTESIAN_POINT('Ctrl Pts',(12.0639368858614,0.0968363912382316,
4.48221150772657));
#29414=CARTESIAN_POINT('Ctrl Pts',(12.1116527219243,-0.353226459651896,
4.34225179773635));
#29415=CARTESIAN_POINT('Ctrl Pts',(12.1593685579871,-0.478916017555994,
3.88799699566402));
#29416=CARTESIAN_POINT('Ctrl Pts',(12.2070843940499,-0.164809627468288,
3.53659627586117));
#29417=CARTESIAN_POINT('Ctrl Pts',(12.2548002301128,0.300643979445627,3.61074632631782));
#29418=CARTESIAN_POINT('Ctrl Pts',(12.3025160661756,0.490011594032383,4.04235401475446));
#29419=CARTESIAN_POINT('Ctrl Pts',(12.3502319022385,0.229394022021679,4.43506735974179));
#29420=CARTESIAN_POINT('Ctrl Pts',(12.3979477383013,-0.241879610092261,
4.42825165390643));
#29421=CARTESIAN_POINT('Ctrl Pts',(12.4456635743641,-0.491031474462283,
4.0281658647901));
#29422=CARTESIAN_POINT('Ctrl Pts',(12.493379410427,-0.289261580343189,3.60221492864948));
#29423=CARTESIAN_POINT('Ctrl Pts',(12.5410952464898,0.178141673866572,3.54155614424011));
#29424=CARTESIAN_POINT('Ctrl Pts',(12.5888110825527,0.481954687902679,3.90189340664049));
#29425=CARTESIAN_POINT('Ctrl Pts',(12.6365269186155,0.343181296211668,4.35232346328687));
#29426=CARTESIAN_POINT('Ctrl Pts',(12.6842427546783,-0.110740760313508,
4.47920946240362));
#29427=CARTESIAN_POINT('Ctrl Pts',(12.7319585907412,-0.462967872677167,
4.16603003860975));
#29428=CARTESIAN_POINT('Ctrl Pts',(12.779674426804,-0.390044463885,3.70038267566003));
#29429=CARTESIAN_POINT('Ctrl Pts',(12.8273902628668,0.0410627776982723,
3.50987851185683));
#29430=CARTESIAN_POINT('Ctrl Pts',(12.8751060989297,0.434461438689172,3.76946045210395));
#29431=CARTESIAN_POINT('Ctrl Pts',(12.9228219349925,0.42888747548329,4.24075040649094));
#29432=CARTESIAN_POINT('Ctrl Pts',(12.9705377710553,0.0294595442590321,
4.49095555817611));
#29433=CARTESIAN_POINT('Ctrl Pts',(13.0182536071182,-0.397021539751646,
4.29030866646591));
#29434=CARTESIAN_POINT('Ctrl Pts',(13.065969443181,-0.458911634846768,3.82306685936703));
#29435=CARTESIAN_POINT('Ctrl Pts',(13.1136852792439,-0.0993761143989603,
3.51830547777773));
#29436=CARTESIAN_POINT('Ctrl Pts',(13.1614011153067,0.351418020999476,3.65589158776806));
#29437=CARTESIAN_POINT('Ctrl Pts',(13.2091169513695,0.479499580452807,4.10947774749948));
#29438=CARTESIAN_POINT('Ctrl Pts',(13.2568327874324,0.167249297126924,4.46252880717046));
#29439=CARTESIAN_POINT('Ctrl Pts',(13.3045486234952,-0.298588589211839,
4.39083254629632));
#29440=CARTESIAN_POINT('Ctrl Pts',(13.352264459558,-0.490227979701372,3.96022874442655));
#29441=CARTESIAN_POINT('Ctrl Pts',(13.3999802956209,-0.23168347330409,3.56614749850931));
#29442=CARTESIAN_POINT('Ctrl Pts',(13.4476961316837,0.239619531536799,3.57047968038978));
#29443=CARTESIAN_POINT('Ctrl Pts',(13.4954119677466,0.490876233547033,3.96924698078795));
#29444=CARTESIAN_POINT('Ctrl Pts',(13.5431278038094,0.291353737189313,4.39625525192456));
#29445=CARTESIAN_POINT('Ctrl Pts',(13.5908436398722,-0.175723379082843,
4.45937622804808));
#29446=CARTESIAN_POINT('Ctrl Pts',(13.6385594759351,-0.481431012491488,
4.10064494554323));
#29447=CARTESIAN_POINT('Ctrl Pts',(13.6862753119979,-0.345033139360895,
3.64948986092447));
#29448=CARTESIAN_POINT('Ctrl Pts',(13.7339911480608,0.108213974662067,3.52021363031051));
#29449=CARTESIAN_POINT('Ctrl Pts',(13.7817069841236,0.462086530666827,3.83153260544464));
#29450=CARTESIAN_POINT('Ctrl Pts',(13.8294228201864,0.391617915445045,4.297557781203));
#29451=CARTESIAN_POINT('Ctrl Pts',(13.8771386562493,-0.0384794573460961,
4.49033106796769));
#29452=CARTESIAN_POINT('Ctrl Pts',(13.9248544923121,-0.433240552373761,
4.23282579030437));
#29453=CARTESIAN_POINT('Ctrl Pts',(13.9725703283749,-0.430150181893835,
3.76151300691929));
#29454=CARTESIAN_POINT('Ctrl Pts',(14.0202861644378,-0.032046280669499,
3.50920649887429));
#29455=CARTESIAN_POINT('Ctrl Pts',(14.0680020005006,0.39548621318905,3.70760321474174));
#29456=CARTESIAN_POINT('Ctrl Pts',(14.1157178365634,0.459837632138507,4.1745123976147));
#29457=CARTESIAN_POINT('Ctrl Pts',(14.1634336726263,0.101913077983734,4.48116416053968));
#29458=CARTESIAN_POINT('Ctrl Pts',(14.2111495086891,-0.349599823817769,
4.34595547117883));
#29459=CARTESIAN_POINT('Ctrl Pts',(14.258865344752,-0.480069828122688,3.8930505494253));
#29460=CARTESIAN_POINT('Ctrl Pts',(14.3065811808148,-0.169684322438749,
3.53835895376334));
#29461=CARTESIAN_POINT('Ctrl Pts',(14.3542970168777,0.296524907469595,3.60759943412104));
#29462=CARTESIAN_POINT('Ctrl Pts',(14.4020128529405,0.49043075222644,4.0371873919842));
#29463=CARTESIAN_POINT('Ctrl Pts',(14.4497286890033,0.233966490966644,4.43262559558668));
#29464=CARTESIAN_POINT('Ctrl Pts',(14.4974445250662,-0.237352798985028,
4.43077705796148));
#29465=CARTESIAN_POINT('Ctrl Pts',(14.545160361129,-0.490707361486496,4.03333931965322));
#29466=CARTESIAN_POINT('Ctrl Pts',(14.5928761971918,-0.293437803431633,
3.60528557111603));
#29467=CARTESIAN_POINT('Ctrl Pts',(14.6405920332547,0.173300204635467,3.53970415608515));
#29468=CARTESIAN_POINT('Ctrl Pts',(14.6883078693175,0.480893968219416,3.89681949708321));
#29469=CARTESIAN_POINT('Ctrl Pts',(14.7360237053804,0.346875401282657,4.34868708154587));
#29470=CARTESIAN_POINT('Ctrl Pts',(14.7837395414432,-0.10568418401607,4.48034995378457));
#29471=CARTESIAN_POINT('Ctrl Pts',(14.831455377506,-0.461192356972643,4.17090007232882));
#29472=CARTESIAN_POINT('Ctrl Pts',(14.8791712135689,-0.393180492164677,
3.7045100248179));
#29473=CARTESIAN_POINT('Ctrl Pts',(14.9268870496317,0.0358950684576197,
3.50947296821438));
#29474=CARTESIAN_POINT('Ctrl Pts',(14.9746028856945,0.432007635398663,3.76489443262817));
#29475=CARTESIAN_POINT('Ctrl Pts',(15.0223187217574,0.431400943461215,4.23621695712364));
#29476=CARTESIAN_POINT('Ctrl Pts',(15.0700345578202,0.0346321271865876,
4.4906178152274));
#29477=CARTESIAN_POINT('Ctrl Pts',(15.1177503938831,-0.393939904367254,
4.2944767844824));
#29478=CARTESIAN_POINT('Ctrl Pts',(15.1654662299459,-0.46075086019608,3.82791319143947));
#29479=CARTESIAN_POINT('Ctrl Pts',(15.2131820660087,-0.104447211543591,
3.51937956259357));
#29480=CARTESIAN_POINT('Ctrl Pts',(15.2608979020716,0.347771918596306,3.652207076714));
#29481=CARTESIAN_POINT('Ctrl Pts',(15.3086137381344,0.480626744730421,4.10441818376995));
#29482=CARTESIAN_POINT('Ctrl Pts',(15.3563295741973,0.172114635785536,4.46074046598969));
#29483=CARTESIAN_POINT('Ctrl Pts',(15.4040454102601,-0.294452991525291,
4.39395768888776));
#29484=CARTESIAN_POINT('Ctrl Pts',(15.4517612463229,-0.490619905976795,
3.96539750426199));
#29485=CARTESIAN_POINT('Ctrl Pts',(15.4994770823858,-0.236243011612202,
3.56861332390027));
#29486=CARTESIAN_POINT('Ctrl Pts',(15.5471929184486,0.235079475381852,3.56797816593814));
#29487=CARTESIAN_POINT('Ctrl Pts',(15.5949087545115,0.490524862970081,3.9640753057054));
#29488=CARTESIAN_POINT('Ctrl Pts',(15.6426245905743,0.295513721197704,4.39316264501585));
#29489=CARTESIAN_POINT('Ctrl Pts',(15.6903404266371,-0.170872217813597,
4.46120267782338));
#29490=CARTESIAN_POINT('Ctrl Pts',(15.7380562626999,-0.480343569999647,
4.1057131950703));
#29491=CARTESIAN_POINT('Ctrl Pts',(15.7857720987628,-0.348708030819167,
3.6531456586776));
#29492=CARTESIAN_POINT('Ctrl Pts',(15.8334879348256,0.103151458625294,3.5190998009613));
#29493=CARTESIAN_POINT('Ctrl Pts',(15.8812037708885,0.460285376424935,3.82667199562295));
#29494=CARTESIAN_POINT('Ctrl Pts',(15.9289196069513,0.39473215065269,4.29341396369818));
#29495=CARTESIAN_POINT('Ctrl Pts',(15.9766354430142,-0.033309682798763,
4.49070937415524));
#29496=CARTESIAN_POINT('Ctrl Pts',(16.024351279077,-0.430762722000766,4.23737881579128));
#29497=CARTESIAN_POINT('Ctrl Pts',(16.0720671151398,-0.432639725453012,
3.76605963834362));
#29498=CARTESIAN_POINT('Ctrl Pts',(16.1197829512026,-0.0372170120039125,
3.50957149464017));
#29499=CARTESIAN_POINT('Ctrl Pts',(16.1674987872655,0.392382656225717,3.70345139362117));
#29500=CARTESIAN_POINT('Ctrl Pts',(16.2152146233283,0.461651293660056,4.16965644082667));
#29501=CARTESIAN_POINT('Ctrl Pts',(16.2629304593912,0.106978444708158,4.48006336792116));
#29502=CARTESIAN_POINT('Ctrl Pts',(16.310646295454,-0.345934356094203,4.34962071752925));
#29503=CARTESIAN_POINT('Ctrl Pts',(16.3583621315169,-0.481170314810987,
3.89811598262401));
#29504=CARTESIAN_POINT('Ctrl Pts',(16.4060779675797,-0.174540169679895,
3.54017290856226));
#29505=CARTESIAN_POINT('Ctrl Pts',(16.4537938036425,0.292372898913969,3.60449612791703));
#29506=CARTESIAN_POINT('Ctrl Pts',(16.5015096397054,0.490795435699827,4.0320166386149));
#29507=CARTESIAN_POINT('Ctrl Pts',(16.5492254757682,0.238512972024049,4.4301357774334));
#29508=CARTESIAN_POINT('Ctrl Pts',(16.596941311831,-0.23279962385521,4.43325461334514));
#29509=CARTESIAN_POINT('Ctrl Pts',(16.6446571478939,-0.490328743065594,
4.03850907134293));
#29510=CARTESIAN_POINT('Ctrl Pts',(16.6923729839567,-0.297581432841348,
3.60840005658827));
#29511=CARTESIAN_POINT('Ctrl Pts',(16.7400888200196,0.168439486040012,3.53790329540825));
#29512=CARTESIAN_POINT('Ctrl Pts',(16.7878046560824,0.479779833116189,3.89175704832657));
#29513=CARTESIAN_POINT('Ctrl Pts',(16.8355204921452,0.350530977080134,4.3450119692985));
#29514=CARTESIAN_POINT('Ctrl Pts',(16.8832363282081,-0.100615868820984,
4.4814370901721));
#29515=CARTESIAN_POINT('Ctrl Pts',(16.9309521642709,-0.459365614209645,
4.17575112327883));
#29516=CARTESIAN_POINT('Ctrl Pts',(16.9786680003337,-0.396272847821079,
3.70867019559999));
#29517=CARTESIAN_POINT('Ctrl Pts',(17.0263838363966,0.0307233721630972,
3.5091219099869));
#29518=CARTESIAN_POINT('Ctrl Pts',(17.0740996724594,0.429505846750062,3.76035452756312));
#29519=CARTESIAN_POINT('Ctrl Pts',(17.1218155085223,0.433866493469502,4.23165726989771));
#29520=CARTESIAN_POINT('Ctrl Pts',(17.1695313445851,0.039800863341802,4.49022557677993));
#29521=CARTESIAN_POINT('Ctrl Pts',(17.217247180648,-0.390814512007675,4.29861219341511));
#29522=CARTESIAN_POINT('Ctrl Pts',(17.2649630167107,-0.462538907526291,
3.83277863809798));
#29523=CARTESIAN_POINT('Ctrl Pts',(17.3126788527736,-0.109506707187599,
3.52050703244687));
#29524=CARTESIAN_POINT('Ctrl Pts',(17.3603946888365,0.344087187338735,3.64856119684745));
#29525=CARTESIAN_POINT('Ctrl Pts',(17.4081105248993,0.481700523269991,4.09934702176407));
#29526=CARTESIAN_POINT('Ctrl Pts',(17.4558263609621,0.176960856767158,4.45890094794434));
#29527=CARTESIAN_POINT('Ctrl Pts',(17.503542197025,-0.290284687397741,4.39703907252861));
#29528=CARTESIAN_POINT('Ctrl Pts',(17.5512580330878,-0.490957336521241,
3.97057010757845));
#29529=CARTESIAN_POINT('Ctrl Pts',(17.5989738691507,-0.240776309167652,
3.57112706567612));
#29530=CARTESIAN_POINT('Ctrl Pts',(17.6466897052135,0.230513307714322,3.56552463842171));
#29531=CARTESIAN_POINT('Ctrl Pts',(17.6944055412763,0.490119007219086,3.95890762096741));
#29532=CARTESIAN_POINT('Ctrl Pts',(17.7421213773392,0.299640880944266,4.39002636746625));
#29533=CARTESIAN_POINT('Ctrl Pts',(17.789837213402,-0.166002076869247,4.46297789939377));
#29534=CARTESIAN_POINT('Ctrl Pts',(17.8375530494648,-0.479202773223469,
4.11076970247734));
#29535=CARTESIAN_POINT('Ctrl Pts',(17.8852688855277,-0.352344189444135,
3.65683998336499));
#29536=CARTESIAN_POINT('Ctrl Pts',(17.9329847215905,0.0980774850139738,
3.51803938772416));
#29537=CARTESIAN_POINT('Ctrl Pts',(17.9807005576534,0.458433095867658,3.82183063825345));
#29538=CARTESIAN_POINT('Ctrl Pts',(18.0284163937162,0.397802540886209,4.28923755516265));
#29539=CARTESIAN_POINT('Ctrl Pts',(18.076132229779,-0.0281362083699241,
4.49103317467411));
#29540=CARTESIAN_POINT('Ctrl Pts',(18.1238480658419,-0.428237044548737,
4.24190547436581));
#29541=CARTESIAN_POINT('Ctrl Pts',(18.1715639019047,-0.435081213444543,
3.7706322547532));
#29542=CARTESIAN_POINT('Ctrl Pts',(18.2192797379675,-0.0423836094492617,
3.50999096487715));
#29543=CARTESIAN_POINT('Ctrl Pts',(18.2669955740304,0.389235515258945,3.69933251171255));
#29544=CARTESIAN_POINT('Ctrl Pts',(18.3147114100932,0.463413677146622,4.16478163940629));
#29545=CARTESIAN_POINT('Ctrl Pts',(18.3624272461561,0.112031928774586,4.4789092521418));
#29546=CARTESIAN_POINT('Ctrl Pts',(18.4101430822189,-0.342230463623947,
4.35324712966946));
#29547=CARTESIAN_POINT('Ctrl Pts',(18.4578589182817,-0.482217355384067,
3.90319273261591));
#29548=CARTESIAN_POINT('Ctrl Pts',(18.5055747543446,-0.179376629827252,
3.54203793877243));
#29549=CARTESIAN_POINT('Ctrl Pts',(18.5532905904074,0.288188414964166,3.60143675240633));
#29550=CARTESIAN_POINT('Ctrl Pts',(18.6010064264702,0.491105603945206,4.02684232898929));
#29551=CARTESIAN_POINT('Ctrl Pts',(18.6487222625331,0.243032960192409,4.42759818183915));
#29552=CARTESIAN_POINT('Ctrl Pts',(18.6964380985959,-0.228220590447982,
4.43568404486223));
#29553=CARTESIAN_POINT('Ctrl Pts',(18.7441539346588,-0.489895661254576,
4.0436745456279));
#29554=CARTESIAN_POINT('Ctrl Pts',(18.7918697707216,-0.301692008317894,
3.6115580391236));
#29555=CARTESIAN_POINT('Ctrl Pts',(18.8395856067845,0.163560057986223,3.53615376224111));
#29556=CARTESIAN_POINT('Ctrl Pts',(18.8873014428472,0.478612406344963,3.88670662268212));
#29557=CARTESIAN_POINT('Ctrl Pts',(18.9350172789101,0.35414761756175,4.34129853476112));
#29558=CARTESIAN_POINT('Ctrl Pts',(18.982733114973,-0.0955363776958117,
4.48247075080787));
#29559=CARTESIAN_POINT('Ctrl Pts',(19.0304489510358,-0.457487847288108,
4.18058265263639));
#29560=CARTESIAN_POINT('Ctrl Pts',(19.0781647870987,-0.399321187381313,
3.71286272589862));
#29561=CARTESIAN_POINT('Ctrl Pts',(19.1258806231614,0.0255482632835279,
3.50882537619781));
#29562=CARTESIAN_POINT('Ctrl Pts',(19.1735964592243,0.426956350589889,3.75584124112414));
#29563=CARTESIAN_POINT('Ctrl Pts',(19.2213122952871,0.436283851722622,4.22707185138688));
#29564=CARTESIAN_POINT('Ctrl Pts',(19.26902813135,0.0449651784623906,4.48977888620274));
#29565=CARTESIAN_POINT('Ctrl Pts',(19.3167439674128,-0.387645709555542,
4.3027144342981));
#29566=CARTESIAN_POINT('Ctrl Pts',(19.3644598034757,-0.464275578741542,
3.8376626582024));
#29567=CARTESIAN_POINT('Ctrl Pts',(19.4121756395385,-0.114554038379521,
3.52168776344319));
#29568=CARTESIAN_POINT('Ctrl Pts',(19.4598914756013,0.340364234683876,3.64495435060606));
#29569=CARTESIAN_POINT('Ctrl Pts',(19.5076073116642,0.482720800247919,4.09426482953845));
#29570=CARTESIAN_POINT('Ctrl Pts',(19.555323147727,0.181787415268628,4.45701044834135));
#29571=CARTESIAN_POINT('Ctrl Pts',(19.6030389837899,-0.28608412753634,4.40007637198121));
#29572=CARTESIAN_POINT('Ctrl Pts',(19.6507548198527,-0.491240257057309,
3.97574594767572));
#29573=CARTESIAN_POINT('Ctrl Pts',(19.6984706559155,-0.245282818621706,
3.57368850533185));
#29574=CARTESIAN_POINT('Ctrl Pts',(19.7461864919783,0.225921452997342,3.56311925573479));
#29575=CARTESIAN_POINT('Ctrl Pts',(19.7939023280412,0.489658867576397,3.95374471702426));
#29576=CARTESIAN_POINT('Ctrl Pts',(19.841618164104,0.303734463062876,4.38684635894002));
#29577=CARTESIAN_POINT('Ctrl Pts',(19.8893340001669,-0.161112940293692,
4.46470246728215));
#29578=CARTESIAN_POINT('Ctrl Pts',(19.9370498362297,-0.47800980043334,4.11581244897344));
#29579=CARTESIAN_POINT('Ctrl Pts',(19.9847656722926,-0.355939225796451,
3.66057517601247));
#29580=CARTESIAN_POINT('Ctrl Pts',(20.0324815083554,0.0929888682922082,
3.51702731322357));
#29581=CARTESIAN_POINT('Ctrl Pts',(20.0801973444182,0.456536973876988,3.81701888067549));
#29582=CARTESIAN_POINT('Ctrl Pts',(20.1279131804811,0.400815378068436,4.28501049648274));
#29583=CARTESIAN_POINT('Ctrl Pts',(20.1756290165439,-0.022934367574535,
4.49133741301101));
#29584=CARTESIAN_POINT('Ctrl Pts',(20.2233448526067,-0.425711472830213,
4.24633918020534));
#29585=CARTESIAN_POINT('Ctrl Pts',(20.2710606886696,-0.437384262562023,
3.77535541015343));
#29586=CARTESIAN_POINT('Ctrl Pts',(20.3187765247324,-0.0477164433392854,
3.51022640082505));
#29587=CARTESIAN_POINT('Ctrl Pts',(20.3664923607953,0.386374384143037,3.69571627142296));
#29588=CARTESIAN_POINT('Ctrl Pts',(20.4062555575143,0.45143962727185,4.08165775845481));
#29589=CARTESIAN_POINT('Ctrl Pts',(20.4380661148895,0.291471375703242,4.31996082336987));
#29590=CARTESIAN_POINT('Ctrl Pts',(20.461924032921,0.103697252552815,4.42124466395835));
#29591=CARTESIAN_POINT('Ctrl Pts',(20.4857819509523,-0.111451542568667,
4.41901444157942));
#29592=CARTESIAN_POINT('Ctrl Pts',(20.5096398689838,-0.298255971346869,
4.31460392554555));
#29593=CARTESIAN_POINT('Ctrl Pts',(20.5334977870152,-0.412709509332759,
4.13311446574462));
#29594=CARTESIAN_POINT('Ctrl Pts',(20.5573557050466,-0.425936384696969,
3.91915434697803));
#29595=CARTESIAN_POINT('Ctrl Pts',(20.581213623078,-0.335173342752607,3.72492109335083));
#29596=CARTESIAN_POINT('Ctrl Pts',(20.6050715411095,-0.162364888615448,
3.59797442377207));
#29597=CARTESIAN_POINT('Ctrl Pts',(20.6289294591408,0.0501004451364318,
3.56932214892951));
#29598=CARTESIAN_POINT('Ctrl Pts',(20.6527873771723,0.250339089241223,3.64598859455508));
#29599=CARTESIAN_POINT('Ctrl Pts',(20.6766452952037,0.389350172549011,3.80921715950176));
#29600=CARTESIAN_POINT('Ctrl Pts',(20.7005032132352,0.433161330121289,4.01909908002448));
#29601=CARTESIAN_POINT('Ctrl Pts',(20.7243611312665,0.371049143609512,4.22430982617278));
#29602=CARTESIAN_POINT('Ctrl Pts',(20.748219049298,0.218207240773441,4.37467120177868));
#29603=CARTESIAN_POINT('Ctrl Pts',(20.7720769673293,0.01200671405148,4.43341500212799));
#29604=CARTESIAN_POINT('Ctrl Pts',(20.7959348853608,-0.197129246586683,
4.38617716647524));
#29605=CARTESIAN_POINT('Ctrl Pts',(20.8197928033922,-0.358062019934396,
4.24450842127602));
#29606=CARTESIAN_POINT('Ctrl Pts',(20.8436507214237,-0.431438726014498,
4.04305074550709));
#29607=CARTESIAN_POINT('Ctrl Pts',(20.867508639455,-0.399316990859146,3.83106596928302));
#29608=CARTESIAN_POINT('Ctrl Pts',(20.8913665574865,-0.269551332195825,
3.66039017609669));
#29609=CARTESIAN_POINT('Ctrl Pts',(20.9152244755179,-0.0738730526583281,
3.57275822989076));
#29610=CARTESIAN_POINT('Ctrl Pts',(20.9390823935493,0.139869212314499,3.58959853735383));
#29611=CARTESIAN_POINT('Ctrl Pts',(20.9629403115807,0.319409638666883,3.70679317993256));
#29612=CARTESIAN_POINT('Ctrl Pts',(20.9867982296122,0.420845711130686,3.8956848776653));
#29613=CARTESIAN_POINT('Ctrl Pts',(21.0106561476436,0.419373541863394,4.11008446384341));
#29614=CARTESIAN_POINT('Ctrl Pts',(21.034514065675,0.315353119032788,4.29756540021079));
#29615=CARTESIAN_POINT('Ctrl Pts',(21.0583719837064,0.134220268060588,4.41228349058099));
#29616=CARTESIAN_POINT('Ctrl Pts',(21.0822299017379,-0.079733094278782,
4.42618703719455));
#29617=CARTESIAN_POINT('Ctrl Pts',(21.1060878197692,-0.274189543318984,
4.33587624407661));
#29618=CARTESIAN_POINT('Ctrl Pts',(21.1299457378007,-0.401599180171465,
4.16343456021562));
#29619=CARTESIAN_POINT('Ctrl Pts',(21.1538036558321,-0.430806878168669,
3.95102867450389));
#29620=CARTESIAN_POINT('Ctrl Pts',(21.1776615738635,-0.354670559489406,
3.75059761183336));
#29621=CARTESIAN_POINT('Ctrl Pts',(21.2015194918949,-0.191807627993766,
3.61115222665144));
#29622=CARTESIAN_POINT('Ctrl Pts',(21.2253774099264,0.0179574932869785,
3.56679071405539));
#29623=CARTESIAN_POINT('Ctrl Pts',(21.2492353279577,0.223331518303719,3.62836067225603));
#29624=CARTESIAN_POINT('Ctrl Pts',(21.2730932459892,0.374094903668402,3.78080656934254));
#29625=CARTESIAN_POINT('Ctrl Pts',(21.2969511640206,0.433381894944723,3.98685123093373));
#29626=CARTESIAN_POINT('Ctrl Pts',(21.320809082052,0.386695207821707,4.19611112472705));
#29627=CARTESIAN_POINT('Ctrl Pts',(21.3446670000834,0.245451009020076,4.35741650656472));
#29628=CARTESIAN_POINT('Ctrl Pts',(21.3685249181149,0.0441873525619181,
4.43132381671722));
#29629=CARTESIAN_POINT('Ctrl Pts',(21.3923828361462,-0.167881315237013,
4.39976070465745));
#29630=CARTESIAN_POINT('Ctrl Pts',(21.4162407541777,-0.338898428465248,
4.27044521104599));
#29631=CARTESIAN_POINT('Ctrl Pts',(21.4400986722091,-0.427045644525908,
4.07499849655415));
#29632=CARTESIAN_POINT('Ctrl Pts',(21.4639565902406,-0.410768568010174,
3.86121260673678));
#29633=CARTESIAN_POINT('Ctrl Pts',(21.4878145082719,-0.294047387504818,
3.68136401506497));
#29634=CARTESIAN_POINT('Ctrl Pts',(21.5116724263034,-0.105423611064507,
3.57943060117972));
#29635=CARTESIAN_POINT('Ctrl Pts',(21.5355303443348,0.108979109962582,3.58033786138646));
#29636=CARTESIAN_POINT('Ctrl Pts',(21.5593882623662,0.296733470072461,3.68386394585134));
#29637=CARTESIAN_POINT('Ctrl Pts',(21.5832461803976,0.411928413892185,3.86469390692879));
#29638=CARTESIAN_POINT('Ctrl Pts',(21.6071040984291,0.426395639810567,4.07860989342611));
#29639=CARTESIAN_POINT('Ctrl Pts',(21.6309620164605,0.33659751701124,4.27330361969026));
#29640=CARTESIAN_POINT('Ctrl Pts',(21.6548199344919,0.164492132570386,4.401167166299));
#29641=CARTESIAN_POINT('Ctrl Pts',(21.6786778525233,-0.0478360589596606,
4.43093441317345));
#29642=CARTESIAN_POINT('Ctrl Pts',(21.7025357705547,-0.248467031045983,
4.35532645760922));
#29643=CARTESIAN_POINT('Ctrl Pts',(21.7263936885861,-0.388341045935521,
4.1928315042612));
#29644=CARTESIAN_POINT('Ctrl Pts',(21.7502516066176,-0.433255096896122,
3.98318399549658));
#29645=CARTESIAN_POINT('Ctrl Pts',(21.774109524649,-0.372226475033738,3.77764845789182));
#29646=CARTESIAN_POINT('Ctrl Pts',(21.7979674426804,-0.220178340780001,
3.62648392906691));
#29647=CARTESIAN_POINT('Ctrl Pts',(21.8218253607118,-0.0142906046679706,
3.56665425395863));
#29648=CARTESIAN_POINT('Ctrl Pts',(21.8456832787432,0.195091573553633,3.61278941785858));
#29649=CARTESIAN_POINT('Ctrl Pts',(21.8695411967747,0.356768547853618,3.75360811649661));
#29650=CARTESIAN_POINT('Ctrl Pts',(21.8933991148061,0.431205894023261,3.95467634223136));
#29651=CARTESIAN_POINT('Ctrl Pts',(21.9172570328375,0.400201653291494,4.16682743688221));
#29652=CARTESIAN_POINT('Ctrl Pts',(21.941114950869,0.271337207055788,4.33818467892719));
#29653=CARTESIAN_POINT('Ctrl Pts',(21.9649728689003,0.0761234226178432,
4.4268465550088));
#29654=CARTESIAN_POINT('Ctrl Pts',(21.9888307869318,-0.137704612210607,
4.41113282132402));
#29655=CARTESIAN_POINT('Ctrl Pts',(22.0126887049632,-0.317860118355158,
4.29488591379237));
#29656=CARTESIAN_POINT('Ctrl Pts',(22.0365466229946,-0.420290167226249,
4.10653136780738));
#29657=CARTESIAN_POINT('Ctrl Pts',(22.060404541026,-0.419947821735935,3.89212700053744));
#29658=CARTESIAN_POINT('Ctrl Pts',(22.0842624590574,-0.316916794682727,
3.70410052003731));
#29659=CARTESIAN_POINT('Ctrl Pts',(22.1081203770888,-0.136390978688423,
3.58842952252864));
#29660=CARTESIAN_POINT('Ctrl Pts',(22.1319782951203,0.0774861468089536,
3.57339871771534));
#29661=CARTESIAN_POINT('Ctrl Pts',(22.1558362131517,0.27241579873489,3.66268354680831));
#29662=CARTESIAN_POINT('Ctrl Pts',(22.1796941311831,0.400732367405962,3.83445143701846));
#29663=CARTESIAN_POINT('Ctrl Pts',(22.2035520492145,0.431058956528623,4.04670046033727));
#29664=CARTESIAN_POINT('Ctrl Pts',(22.227409967246,0.355979888945518,4.24752994899471));
#29665=CARTESIAN_POINT('Ctrl Pts',(22.2512678852773,0.193854041863619,4.38783162256878));
#29666=CARTESIAN_POINT('Ctrl Pts',(22.2751258033088,-0.0156743990186396,
4.43329790005389));
#29667=CARTESIAN_POINT('Ctrl Pts',(22.2989837213402,-0.221370022215225,
4.37281103827166));
#29668=CARTESIAN_POINT('Ctrl Pts',(22.3228416393716,-0.372934645290675,
4.22116172228637));
#29669=CARTESIAN_POINT('Ctrl Pts',(22.346699557403,-0.43330658847365,4.01543234121164));
#29670=CARTESIAN_POINT('Ctrl Pts',(22.3705574754345,-0.387723268841402,
3.80592933171158));
#29671=CARTESIAN_POINT('Ctrl Pts',(22.3944153934659,-0.247331046528593,
3.64388188817752));
#29672=CARTESIAN_POINT('Ctrl Pts',(22.4182733114973,-0.0464596501027702,
3.56891502119853));
#29673=CARTESIAN_POINT('Ctrl Pts',(22.4421312295287,0.165772403721094,3.59936017830047));
#29674=CARTESIAN_POINT('Ctrl Pts',(22.4659891475602,0.337468575289321,3.7277726770023));
#29675=CARTESIAN_POINT('Ctrl Pts',(22.4898470655915,0.426644514167594,3.92275218663495));
#29676=CARTESIAN_POINT('Ctrl Pts',(22.513704983623,0.411494197867752,4.13662086224655));
#29677=CARTESIAN_POINT('Ctrl Pts',(22.5375629016544,0.295722435535401,4.31708206952049));
#29678=CARTESIAN_POINT('Ctrl Pts',(22.5614208196858,0.107638304484935,4.42000797176855));
#29679=CARTESIAN_POINT('Ctrl Pts',(22.5852787377172,-0.106765988085903,
4.42023067651324));
#29680=CARTESIAN_POINT('Ctrl Pts',(22.6091366557487,-0.295063722636797,
4.31769517074077));
#29681=CARTESIAN_POINT('Ctrl Pts',(22.6329945737801,-0.411209141905604,
4.13747522778479));
#29682=CARTESIAN_POINT('Ctrl Pts',(22.6568524918115,-0.426804986482714,
3.92363755172126));
#29683=CARTESIAN_POINT('Ctrl Pts',(22.6807104098429,-0.33803111495158,3.72847502015617));
#29684=CARTESIAN_POINT('Ctrl Pts',(22.7045683278743,-0.16660749730952,3.59970312177549));
#29685=CARTESIAN_POINT('Ctrl Pts',(22.7284262459057,0.0455714674079685,
3.56882345794434));
#29686=CARTESIAN_POINT('Ctrl Pts',(22.7522841639372,0.246577802732478,3.64336153500176));
#29687=CARTESIAN_POINT('Ctrl Pts',(22.7761420819686,0.387346815298129,3.80514019809748));
#29688=CARTESIAN_POINT('Ctrl Pts',(22.7920473606562,0.417963038852713,3.94471011778788));
#29689=CARTESIAN_POINT('Ctrl Pts',(22.8,0.415641328671541,4.01393920819689));
#29690=CARTESIAN_POINT('Ctrl Pts',(3.96816317011929,0.203757107801821,4.42939176513376));
#29691=CARTESIAN_POINT('Ctrl Pts',(3.9761158094631,0.132237748973037,4.46332948562603));
#29692=CARTESIAN_POINT('Ctrl Pts',(3.99202108815071,-0.0280119004087947,
4.49474661085258));
#29693=CARTESIAN_POINT('Ctrl Pts',(4.01587900618213,-0.261670681609628,
4.42079217330492));
#29694=CARTESIAN_POINT('Ctrl Pts',(4.03973692421355,-0.431283260509235,
4.24398813071681));
#29695=CARTESIAN_POINT('Ctrl Pts',(4.06359484224497,-0.495466080430727,
4.00749935521381));
#29696=CARTESIAN_POINT('Ctrl Pts',(4.08745276027639,-0.438477829352452,
3.76918881818141));
#29697=CARTESIAN_POINT('Ctrl Pts',(4.11131067830781,-0.274278321106756,
3.5873115455631));
#29698=CARTESIAN_POINT('Ctrl Pts',(4.13516859633923,-0.0430057845205295,
3.50635120590702));
#29699=CARTESIAN_POINT('Ctrl Pts',(4.15902651437064,0.198780450874126,3.54609966156282));
#29700=CARTESIAN_POINT('Ctrl Pts',(4.18288443240206,0.391960715466274,3.69684005745713));
#29701=CARTESIAN_POINT('Ctrl Pts',(4.20674235043348,0.489295238859844,3.92171081754005));
#29702=CARTESIAN_POINT('Ctrl Pts',(4.2306002684649,0.466984102771714,4.16572567991789));
#29703=CARTESIAN_POINT('Ctrl Pts',(4.25445818649632,0.330482445391075,4.36921595913043));
#29704=CARTESIAN_POINT('Ctrl Pts',(4.27831610452774,0.113168927396708,4.48242295331799));
#29705=CARTESIAN_POINT('Ctrl Pts',(4.30217402255916,-0.131817528672551,
4.47766435517297));
#29706=CARTESIAN_POINT('Ctrl Pts',(4.32603194059057,-0.344570980451485,
4.35610383169054));
#29707=CARTESIAN_POINT('Ctrl Pts',(4.349889858622,-0.473067456356951,4.14746621026076));
#29708=CARTESIAN_POINT('Ctrl Pts',(4.37374777665341,-0.485886045261059,
3.9027690893624));
#29709=CARTESIAN_POINT('Ctrl Pts',(4.39760569468484,-0.379892264971952,
3.68184757153936));
#29710=CARTESIAN_POINT('Ctrl Pts',(4.42146361271625,-0.181004475645389,
3.53872299041084));
#29711=CARTESIAN_POINT('Ctrl Pts',(4.44532153074767,0.0621438372772935,
3.50839320219298));
#29712=CARTESIAN_POINT('Ctrl Pts',(4.46917944877909,0.290096289836991,3.5982746675986));
#29713=CARTESIAN_POINT('Ctrl Pts',(4.49303736681051,0.447112297141319,3.78638891931142));
#29714=CARTESIAN_POINT('Ctrl Pts',(4.51689528484194,0.494797168872773,4.02673689903048));
#29715=CARTESIAN_POINT('Ctrl Pts',(4.54075320287334,0.421490654719143,4.26054697856981));
#29716=CARTESIAN_POINT('Ctrl Pts',(4.56461112090478,0.245118194360182,4.43064622472778));
#29717=CARTESIAN_POINT('Ctrl Pts',(4.58846903893618,0.00880765856895839,
4.49544073835303));
#29718=CARTESIAN_POINT('Ctrl Pts',(4.61232695696761,-0.229656589644598,
4.43908649592634));
#29719=CARTESIAN_POINT('Ctrl Pts',(4.63618487499902,-0.411963545977342,
4.2753636447643));
#29720=CARTESIAN_POINT('Ctrl Pts',(4.66004279303045,-0.493534193653132,
4.04430688170513));
#29721=CARTESIAN_POINT('Ctrl Pts',(4.68390071106186,-0.454422287381232,
3.80241587917234));
#29722=CARTESIAN_POINT('Ctrl Pts',(4.70775862909328,-0.304191753628974,
3.60883957626609));
#29723=CARTESIAN_POINT('Ctrl Pts',(4.7316165471247,-0.0795780500979935,
3.51091265195837));
#29724=CARTESIAN_POINT('Ctrl Pts',(4.75547446515612,0.164494654344808,3.53258090671894));
#29725=CARTESIAN_POINT('Ctrl Pts',(4.77933238318754,0.368343935055725,3.66854586202706));
#29726=CARTESIAN_POINT('Ctrl Pts',(4.80319030121895,0.482123090158262,3.88556038269908));
#29727=CARTESIAN_POINT('Ctrl Pts',(4.82704821925038,0.478010016947761,4.13055850707372));
#29728=CARTESIAN_POINT('Ctrl Pts',(4.85090613728179,0.357010473862124,4.34363152012653));
#29729=CARTESIAN_POINT('Ctrl Pts',(4.87476405531322,0.14871214514713,4.47267726617372));
#29730=CARTESIAN_POINT('Ctrl Pts',(4.89862197334463,-0.0959503538938319,
4.48614054517122));
#29731=CARTESIAN_POINT('Ctrl Pts',(4.92247989137606,-0.317150377772593,
4.38072921867179));
#29732=CARTESIAN_POINT('Ctrl Pts',(4.94633780940747,-0.460798495283114,
4.1822192273514));
#29733=CARTESIAN_POINT('Ctrl Pts',(4.97019572743889,-0.49176882879792,3.93915167139151));
#29734=CARTESIAN_POINT('Ctrl Pts',(4.99405364547031,-0.40248828815769,3.71096318925158));
#29735=CARTESIAN_POINT('Ctrl Pts',(5.01791156350173,-0.214788397502062,
3.55345208054429));
#29736=CARTESIAN_POINT('Ctrl Pts',(5.04176948153314,0.0254331070612992,
3.50513410186502));
#29737=CARTESIAN_POINT('Ctrl Pts',(5.06562739956457,0.259435524164246,3.57782431515618));
#29738=CARTESIAN_POINT('Ctrl Pts',(5.08948531759598,0.429998888727244,3.75374798322641));
#29739=CARTESIAN_POINT('Ctrl Pts',(5.11334323562741,0.495415812061873,3.98988697716804));
#29740=CARTESIAN_POINT('Ctrl Pts',(5.13720115365882,0.439690074491602,4.2284988806653));
#29741=CARTESIAN_POINT('Ctrl Pts',(5.16105907169025,0.276448136790977,4.41123658365534));
#29742=CARTESIAN_POINT('Ctrl Pts',(5.18491698972166,0.0456070993489057,
4.49341574008204));
#29743=CARTESIAN_POINT('Ctrl Pts',(5.20877490775308,-0.196386116196418,
4.45494130768376));
#29744=CARTESIAN_POINT('Ctrl Pts',(5.2326328257845,-0.390357576881318,4.3052213332044));
#29745=CARTESIAN_POINT('Ctrl Pts',(5.25649074381592,-0.488875976891831,
4.08086642869437));
#29746=CARTESIAN_POINT('Ctrl Pts',(5.28034866184734,-0.467850883838054,
3.83673747961128));
#29747=CARTESIAN_POINT('Ctrl Pts',(5.30420657987876,-0.332423505683668,
3.632530663945));
#29748=CARTESIAN_POINT('Ctrl Pts',(5.32806449791017,-0.115709525355139,
3.5181801106079));
#29749=CARTESIAN_POINT('Ctrl Pts',(5.3519224159416,0.129298585786916,3.52164764473745));
#29750=CARTESIAN_POINT('Ctrl Pts',(5.37578033397301,0.342689670681295,3.64208535978523));
#29751=CARTESIAN_POINT('Ctrl Pts',(5.39963825200445,0.472283796414913,3.85004295376459));
#29752=CARTESIAN_POINT('Ctrl Pts',(5.42349617003584,0.48639166917272,4.09466913029638));
#29753=CARTESIAN_POINT('Ctrl Pts',(5.44735408806728,0.381563529774833,4.31614612573549));
#29754=CARTESIAN_POINT('Ctrl Pts',(5.47121200609869,0.183432713764955,4.46031678178449));
#29755=CARTESIAN_POINT('Ctrl Pts',(5.49506992413012,-0.059552397366927,
4.49192744591021));
#29756=CARTESIAN_POINT('Ctrl Pts',(5.51892784216153,-0.287975325168481,
4.40324844967551));
#29757=CARTESIAN_POINT('Ctrl Pts',(5.54278576019295,-0.445980441674811,
4.21596422322942));
#29758=CARTESIAN_POINT('Ctrl Pts',(5.56664367822437,-0.494931191930538,
3.97587086145358));
#29759=CARTESIAN_POINT('Ctrl Pts',(5.59050159625579,-0.422857784100094,
3.74167773132221));
#29760=CARTESIAN_POINT('Ctrl Pts',(5.61435951428721,-0.247384129650275,
3.57065143242979));
#29761=CARTESIAN_POINT('Ctrl Pts',(5.63821743231862,-0.0114183168777074,
3.50461255354752));
#29762=CARTESIAN_POINT('Ctrl Pts',(5.66207535035005,0.227339585372105,3.55970939936999));
#29763=CARTESIAN_POINT('Ctrl Pts',(5.68593326838146,0.410506766445453,3.72246929038963));
#29764=CARTESIAN_POINT('Ctrl Pts',(5.70979118641288,0.493293861043031,3.9530929995654));
#29765=CARTESIAN_POINT('Ctrl Pts',(5.73364910444431,0.455457169749513,4.19518674831082));
#29766=CARTESIAN_POINT('Ctrl Pts',(5.75750702247572,0.306248793691327,4.38955201985635));
#29767=CARTESIAN_POINT('Ctrl Pts',(5.78136494050715,0.0821542461994931,
4.48866121222712));
#29768=CARTESIAN_POINT('Ctrl Pts',(5.80522285853855,-0.162029253596618,
4.46827942571263));
#29769=CARTESIAN_POINT('Ctrl Pts',(5.82908077656998,-0.366592184898752,
4.33339056701663));
#29770=CARTESIAN_POINT('Ctrl Pts',(5.85293869460139,-0.481513345756758,
4.11697862749145));
#29771=CARTESIAN_POINT('Ctrl Pts',(5.87679661263282,-0.478691368855474,
3.87196223809426));
#29772=CARTESIAN_POINT('Ctrl Pts',(5.90065453066423,-0.358816329143926,
3.65825454842257));
#29773=CARTESIAN_POINT('Ctrl Pts',(5.92451244869565,-0.151200892471453,
3.52811296978032));
#29774=CARTESIAN_POINT('Ctrl Pts',(5.94837036672708,0.093387223403125,3.5133605500302));
#29775=CARTESIAN_POINT('Ctrl Pts',(5.97222828475848,0.315139728168714,3.61760487120619));
#29776=CARTESIAN_POINT('Ctrl Pts',(5.99608620278992,0.459831779670103,3.81535495398299));
#29777=CARTESIAN_POINT('Ctrl Pts',(6.01994412082132,0.492082823488737,4.05825627791571));
#29778=CARTESIAN_POINT('Ctrl Pts',(6.04380203885276,0.404005480250355,4.28691141512903));
#29779=CARTESIAN_POINT('Ctrl Pts',(6.06765995688416,0.21713917558903,4.44541067075535));
#29780=CARTESIAN_POINT('Ctrl Pts',(6.09151787491559,-0.0228261843714051,
4.49499153360272));
#29781=CARTESIAN_POINT('Ctrl Pts',(6.11537579294701,-0.257204988275768,
4.42353981062321));
#29782=CARTESIAN_POINT('Ctrl Pts',(6.13923371097843,-0.428699479426561,
4.24850911946619));
#29783=CARTESIAN_POINT('Ctrl Pts',(6.16309162900984,-0.49534768549136,4.01273373861842));
#29784=CARTESIAN_POINT('Ctrl Pts',(6.18694954704127,-0.440903093044182,
3.77380201544612));
#29785=CARTESIAN_POINT('Ctrl Pts',(6.21080746507268,-0.278582990390117,
3.59026229064107));
#29786=CARTESIAN_POINT('Ctrl Pts',(6.23466538310411,-0.048260127889517,
3.50676273730504));
#29787=CARTESIAN_POINT('Ctrl Pts',(6.25852330113552,0.194087080856728,3.5441598063702));
#29788=CARTESIAN_POINT('Ctrl Pts',(6.28238121916694,0.388553448942855,3.69248145192407));
#29789=CARTESIAN_POINT('Ctrl Pts',(6.30623913719837,0.488798280742691,3.9170164641697));
#29790=CARTESIAN_POINT('Ctrl Pts',(6.33009705522977,0.468067515948433,4.15995908608738));
#29791=CARTESIAN_POINT('Ctrl Pts',(6.36190761260502,0.291040001689194,4.43610431491443));
#29792=CARTESIAN_POINT('Ctrl Pts',(6.40167080932402,-0.143168317426403,
4.54352222151223));
#29793=CARTESIAN_POINT('Ctrl Pts',(6.44938664538688,-0.535165231989368,
4.17285582464912));
#29794=CARTESIAN_POINT('Ctrl Pts',(6.49710248144971,-0.434543251113388,
3.64369891234367));
#29795=CARTESIAN_POINT('Ctrl Pts',(6.54481831751255,0.0645215567551043,
3.4416075490323));
#29796=CARTESIAN_POINT('Ctrl Pts',(6.59253415357539,0.504653900644641,3.75236619672659));
#29797=CARTESIAN_POINT('Ctrl Pts',(6.64024998963822,0.481186238846835,4.29049388273239));
#29798=CARTESIAN_POINT('Ctrl Pts',(6.68796582570107,0.01592709648968,4.56187610740764));
#29799=CARTESIAN_POINT('Ctrl Pts',(6.7356816617639,-0.464005405879062,4.31726850783359));
#29800=CARTESIAN_POINT('Ctrl Pts',(6.78339749782674,-0.517809574500644,
3.78131383674221));
#29801=CARTESIAN_POINT('Ctrl Pts',(6.83111333388957,-0.0961144992151805,
3.44617913151078));
#29802=CARTESIAN_POINT('Ctrl Pts',(6.87882916995242,0.413851019972934,3.61962818876606));
#29803=CARTESIAN_POINT('Ctrl Pts',(6.92654500601525,0.543767061592725,4.14237771887731));
#29804=CARTESIAN_POINT('Ctrl Pts',(6.97426084207809,0.174335412693353,4.53438003016987));
#29805=CARTESIAN_POINT('Ctrl Pts',(7.02197667814094,-0.355192171006393,
4.43565270890428));
#29806=CARTESIAN_POINT('Ctrl Pts',(7.06969251420376,-0.558540766450571,
3.93685892261342));
#29807=CARTESIAN_POINT('Ctrl Pts',(7.11740835026661,-0.248973074301851,
3.49604849518665));
#29808=CARTESIAN_POINT('Ctrl Pts',(7.16512418632944,0.289230577826905,3.51802452284194));
#29809=CARTESIAN_POINT('Ctrl Pts',(7.21284002239229,0.561829257914175,3.98260602935256));
#29810=CARTESIAN_POINT('Ctrl Pts',(7.26055585845511,0.318491529052478,4.46316069626365));
#29811=CARTESIAN_POINT('Ctrl Pts',(7.30827169451797,-0.217321894570402,
4.51838776411367));
#29812=CARTESIAN_POINT('Ctrl Pts',(7.35598753058078,-0.553565266295818,
4.09757137442565));
#29813=CARTESIAN_POINT('Ctrl Pts',(7.40370336664365,-0.381461142739227,
3.58715368886071));
#29814=CARTESIAN_POINT('Ctrl Pts',(7.45141920270646,0.140944621146953,3.45585912402047));
#29815=CARTESIAN_POINT('Ctrl Pts',(7.49913503876933,0.533918768911932,3.82425749787944));
#29816=CARTESIAN_POINT('Ctrl Pts',(7.54685087483214,0.436587096747522,4.3540429157916));
#29817=CARTESIAN_POINT('Ctrl Pts',(7.594566710895,-0.0616692246238245,4.5587052763707));
#29818=CARTESIAN_POINT('Ctrl Pts',(7.64228254695782,-0.503293747851232,
4.25029998493175));
#29819=CARTESIAN_POINT('Ctrl Pts',(7.68999838302067,-0.482735878399531,
3.7120403659385));
#29820=CARTESIAN_POINT('Ctrl Pts',(7.7377142190835,-0.0188742238918736,
3.43821850974892));
#29821=CARTESIAN_POINT('Ctrl Pts',(7.78543005514633,0.462319920793015,3.6802892401675));
#29822=CARTESIAN_POINT('Ctrl Pts',(7.83314589120918,0.518958568528469,4.21595528072725));
#29823=CARTESIAN_POINT('Ctrl Pts',(7.88086172727202,0.099029577569048,4.55330626409362));
#29824=CARTESIAN_POINT('Ctrl Pts',(7.92857756333485,-0.411839798232008,
4.38254759143289));
#29825=CARTESIAN_POINT('Ctrl Pts',(7.9762933993977,-0.544510350349916,3.86048957930736));
#29826=CARTESIAN_POINT('Ctrl Pts',(8.02400923546053,-0.177148669371157,
3.466546133148));
#29827=CARTESIAN_POINT('Ctrl Pts',(8.07172507152338,0.352891360472903,3.56248158116143));
#29828=CARTESIAN_POINT('Ctrl Pts',(8.1194409075862,0.558865824063627,4.06019692528064));
#29829=CARTESIAN_POINT('Ctrl Pts',(8.16715674364906,0.251625202160443,4.50263250666582));
#29830=CARTESIAN_POINT('Ctrl Pts',(8.21487257971187,-0.286686714637947,
4.48349292318459));
#29831=CARTESIAN_POINT('Ctrl Pts',(8.26258841577472,-0.561729810142263,
4.02035434884804));
#29832=CARTESIAN_POINT('Ctrl Pts',(8.31030425183756,-0.32092777766878,3.53852406277244));
#29833=CARTESIAN_POINT('Ctrl Pts',(8.3580200879004,0.21458717114652,3.4804742305729));
#29834=CARTESIAN_POINT('Ctrl Pts',(8.40573592396324,0.553043418849938,3.89951290636976));
#29835=CARTESIAN_POINT('Ctrl Pts',(8.45345176002607,0.383631385356639,4.41083042643994));
#29836=CARTESIAN_POINT('Ctrl Pts',(8.50116759608892,-0.13807525223727,4.54487604447167));
#29837=CARTESIAN_POINT('Ctrl Pts',(8.54888343215175,-0.532985261140852,
4.17855360686946));
#29838=CARTESIAN_POINT('Ctrl Pts',(8.59659926821459,-0.43844670370641,3.64826264467864));
#29839=CARTESIAN_POINT('Ctrl Pts',(8.64431510427743,0.0587242081113278,
3.4409775080543));
#29840=CARTESIAN_POINT('Ctrl Pts',(8.69203094034026,0.501967776032349,3.74705132745037));
#29841=CARTESIAN_POINT('Ctrl Pts',(8.73974677640311,0.484246611455832,4.28541180496438));
#29842=CARTESIAN_POINT('Ctrl Pts',(8.78746261246592,0.021834332487559,4.56167423035448));
#29843=CARTESIAN_POINT('Ctrl Pts',(8.83517844852879,-0.460628749968427,
4.32214256754115));
#29844=CARTESIAN_POINT('Ctrl Pts',(8.88289428459161,-0.520089363644054,
3.78678242815423));
#29845=CARTESIAN_POINT('Ctrl Pts',(8.93061012065447,-0.101943912081849,
3.44722326576734));
#29846=CARTESIAN_POINT('Ctrl Pts',(8.97832595671729,0.409818202553832,3.61528748398963));
#29847=CARTESIAN_POINT('Ctrl Pts',(9.02604179278014,0.545237955920739,4.1366391252272));
#29848=CARTESIAN_POINT('Ctrl Pts',(9.07375762884296,0.179957304801303,4.53251295530543));
#29849=CARTESIAN_POINT('Ctrl Pts',(9.12147346490582,-0.350580908316224,
4.43937194476168));
#29850=CARTESIAN_POINT('Ctrl Pts',(9.16918930096864,-0.559175278946307,
3.94274891673689));
#29851=CARTESIAN_POINT('Ctrl Pts',(9.21690513703149,-0.254270386902387,
3.49870043939378));
#29852=CARTESIAN_POINT('Ctrl Pts',(9.26462097309432,0.284134913886797,3.51500306204057));
#29853=CARTESIAN_POINT('Ctrl Pts',(9.31233680915716,0.56161475127612,3.97668583545263));
#29854=CARTESIAN_POINT('Ctrl Pts',(9.36005264522,0.323355121014866,4.45977836490307));
#29855=CARTESIAN_POINT('Ctrl Pts',(9.40776848128284,-0.211846492332409,
4.52064934726353));
#29856=CARTESIAN_POINT('Ctrl Pts',(9.45548431734568,-0.552506212093558,
4.10340002281193));
#29857=CARTESIAN_POINT('Ctrl Pts',(9.50320015340851,-0.385790975888367,
3.59119686639829));
#29858=CARTESIAN_POINT('Ctrl Pts',(9.55091598947136,0.135202049632292,3.45440391781584));
#29859=CARTESIAN_POINT('Ctrl Pts',(9.59863182553417,0.532036952624682,3.81864024657791));
#29860=CARTESIAN_POINT('Ctrl Pts',(9.64634766159704,0.440294135581046,4.34942202748599));
#29861=CARTESIAN_POINT('Ctrl Pts',(9.69406349765985,-0.0557775609627595,
4.55932418400469));
#29862=CARTESIAN_POINT('Ctrl Pts',(9.74177933372271,-0.500627865026369,
4.25559033604309));
#29863=CARTESIAN_POINT('Ctrl Pts',(9.78949516978553,-0.485743897486414,
3.71714394973028));
#29864=CARTESIAN_POINT('Ctrl Pts',(9.83721100584839,-0.0247938347541151,
3.43844862667992));
#29865=CARTESIAN_POINT('Ctrl Pts',(9.88492684191122,0.458924787935076,3.67543457032792));
#29866=CARTESIAN_POINT('Ctrl Pts',(9.93264267797406,0.521205716397956,4.21047394212484));
#29867=CARTESIAN_POINT('Ctrl Pts',(9.98035851403688,0.104855415711801,4.55223185431066));
#29868=CARTESIAN_POINT('Ctrl Pts',(10.0280743500997,-0.407785226630454,
4.3868667575037));
#29869=CARTESIAN_POINT('Ctrl Pts',(10.0757901861625,-0.54595042077573,3.86623596457089));
#29870=CARTESIAN_POINT('Ctrl Pts',(10.1235060222254,-0.182760942995651,
3.46844274359687));
#29871=CARTESIAN_POINT('Ctrl Pts',(10.1712218582882,0.34826072087591,3.55878673023755));
#29872=CARTESIAN_POINT('Ctrl Pts',(10.2189376943511,0.559469206087141,4.05430365143988));
#29873=CARTESIAN_POINT('Ctrl Pts',(10.2666535304139,0.256908510808291,4.49995269395588));
#29874=CARTESIAN_POINT('Ctrl Pts',(10.3143693664768,-0.281575222991369,
4.4864874848512));
#29875=CARTESIAN_POINT('Ctrl Pts',(10.3620852025396,-0.561484096926345,
4.02627333283551));
#29876=CARTESIAN_POINT('Ctrl Pts',(10.4098010386024,-0.325773485110519,
3.5419319750098));
#29877=CARTESIAN_POINT('Ctrl Pts',(10.4575168746653,0.209099930751681,3.47824153281512));
#29878=CARTESIAN_POINT('Ctrl Pts',(10.5052327107281,0.55195366278862,3.89368991932227));
#29879=CARTESIAN_POINT('Ctrl Pts',(10.552948546791,0.387939853388008,4.40676448870664));
#29880=CARTESIAN_POINT('Ctrl Pts',(10.6006643828538,-0.13232509260073,4.54630096923553));
#29881=CARTESIAN_POINT('Ctrl Pts',(10.6483802189166,-0.531073869970951,
4.18416086379456));
#29882=CARTESIAN_POINT('Ctrl Pts',(10.6960960549795,-0.442129340924997,
3.6529030034519));
#29883=CARTESIAN_POINT('Ctrl Pts',(10.7438118910423,0.0528293649267388,
3.44038965581316));
#29884=CARTESIAN_POINT('Ctrl Pts',(10.7915277271051,0.499274052081986,3.74177509795313));
#29885=CARTESIAN_POINT('Ctrl Pts',(10.839243563168,0.487227694891584,4.28029244094358));
#29886=CARTESIAN_POINT('Ctrl Pts',(10.8869593992308,0.0277526485205102,
4.56141292256198));
#29887=CARTESIAN_POINT('Ctrl Pts',(10.9346752352937,-0.457208082016334,
4.32697927894352));
#29888=CARTESIAN_POINT('Ctrl Pts',(10.9823910713565,-0.522307595786967,
3.79227553224832));
#29889=CARTESIAN_POINT('Ctrl Pts',(11.0301069074193,-0.107764007611043,
3.44832836054127));
#29890=CARTESIAN_POINT('Ctrl Pts',(11.0778227434822,0.405740926916492,3.61098974390844));
#29891=CARTESIAN_POINT('Ctrl Pts',(11.125538579545,0.54664772512998,4.13088523113667));
#29892=CARTESIAN_POINT('Ctrl Pts',(11.1732544156078,0.185559506100192,4.53058679668394));
#29893=CARTESIAN_POINT('Ctrl Pts',(11.2209702516707,-0.345930862581405,
4.4430423427091));
#29894=CARTESIAN_POINT('Ctrl Pts',(11.2686860877335,-0.559747597323992,
3.94864528834179));
#29895=CARTESIAN_POINT('Ctrl Pts',(11.3164019237964,-0.259539500620097,
3.50140805588402));
#29896=CARTESIAN_POINT('Ctrl Pts',(11.3641177598592,0.279007713031768,3.51203547753114));
#29897=CARTESIAN_POINT('Ctrl Pts',(11.411833595922,0.561337850721073,3.97076822846069));
#29898=CARTESIAN_POINT('Ctrl Pts',(11.4595494319849,0.328182802800164,4.45634496498341));
#29899=CARTESIAN_POINT('Ctrl Pts',(11.5072652680477,-0.206347562673641,
4.52285309839201));
#29900=CARTESIAN_POINT('Ctrl Pts',(11.5549811041106,-0.551385786278872,
4.10921718641821));
#29901=CARTESIAN_POINT('Ctrl Pts',(11.6026969401734,-0.390077958183356,
3.59528545163414));
#29902=CARTESIAN_POINT('Ctrl Pts',(11.6504127762362,0.129444461032819,3.45300931394821));
#29903=CARTESIAN_POINT('Ctrl Pts',(11.6981286122991,0.530096039923511,3.8130431397972));
#29904=CARTESIAN_POINT('Ctrl Pts',(11.7458444483619,0.443952268776438,4.34476232707146));
#29905=CARTESIAN_POINT('Ctrl Pts',(11.7935602844247,-0.0498797018717475,
4.55988096454574));
#29906=CARTESIAN_POINT('Ctrl Pts',(11.8412761204876,-0.497906374793238,
4.26085229740167));
#29907=CARTESIAN_POINT('Ctrl Pts',(11.8889919565504,-0.48869796246776,3.72227895182515));
#29908=CARTESIAN_POINT('Ctrl Pts',(11.9367077926133,-0.0307106916234339,
3.43874111807518));
#29909=CARTESIAN_POINT('Ctrl Pts',(11.9844236286761,0.455478679883424,3.67061595167475));
#29910=CARTESIAN_POINT('Ctrl Pts',(12.0321394647389,0.523394971212992,4.20496922507643));
#29911=CARTESIAN_POINT('Ctrl Pts',(12.0798553008018,0.110669607010866,4.5510961052335));
#29912=CARTESIAN_POINT('Ctrl Pts',(12.1275711368646,-0.403685360180124,
4.39114295225112));
#29913=CARTESIAN_POINT('Ctrl Pts',(12.1752869729274,-0.547329849620031,
3.8719972077086));
#29914=CARTESIAN_POINT('Ctrl Pts',(12.2230028089903,-0.188352916401613,
3.4703983969034));
#29915=CARTESIAN_POINT('Ctrl Pts',(12.2707186450531,0.34359139813055,3.55514088718992));
#29916=CARTESIAN_POINT('Ctrl Pts',(12.318434481116,0.560010444926212,4.04840434580723));
#29917=CARTESIAN_POINT('Ctrl Pts',(12.3661503171788,0.262163283277844,4.49721734887317));
#29918=CARTESIAN_POINT('Ctrl Pts',(12.4138661532417,-0.276432455305192,
4.48942800979656));
#29919=CARTESIAN_POINT('Ctrl Pts',(12.4615819893045,-0.561176016721412,
4.03218939850585));
#29920=CARTESIAN_POINT('Ctrl Pts',(12.5092978253673,-0.330583007179444,
3.54539076726965));
#29921=CARTESIAN_POINT('Ctrl Pts',(12.5570136614301,0.203589464528802,3.47606678951191));
#29922=CARTESIAN_POINT('Ctrl Pts',(12.604729497493,0.550802598333678,3.88787874069406));
#29923=CARTESIAN_POINT('Ctrl Pts',(12.6524453335558,0.392205230901379,4.40265336950419));
#29924=CARTESIAN_POINT('Ctrl Pts',(12.7001611696187,-0.126560234920843,
4.54766521348015));
#29925=CARTESIAN_POINT('Ctrl Pts',(12.7478770056815,-0.529103489635726,
4.18974766500481));
#29926=CARTESIAN_POINT('Ctrl Pts',(12.7955928417443,-0.44576286851447,3.65758191611243));
#29927=CARTESIAN_POINT('Ctrl Pts',(12.8433086778072,0.0469286537069902,
3.43986396243348));
#29928=CARTESIAN_POINT('Ctrl Pts',(12.89102451387,0.496524871139168,3.73652755085263));
#29929=CARTESIAN_POINT('Ctrl Pts',(12.9387403499328,0.490154659387074,4.27514194336855));
#29930=CARTESIAN_POINT('Ctrl Pts',(12.9864561859957,0.0336678819209607,
4.56108925568614));
#29931=CARTESIAN_POINT('Ctrl Pts',(13.0341720220585,-0.45373662956012,4.33177967103923));
#29932=CARTESIAN_POINT('Ctrl Pts',(13.0818878581214,-0.524467812480695,
3.79779170939055));
#29933=CARTESIAN_POINT('Ctrl Pts',(13.1296036941842,-0.113572133225654,
3.44949473238301));
#29934=CARTESIAN_POINT('Ctrl Pts',(13.177319530247,0.401618583502394,3.60673521324049));
#29935=CARTESIAN_POINT('Ctrl Pts',(13.2250353663099,0.547996775303968,4.12511679893576));
#29936=CARTESIAN_POINT('Ctrl Pts',(13.2727512023727,0.191141096329688,4.52860170299893));
#29937=CARTESIAN_POINT('Ctrl Pts',(13.3204670384356,-0.341242392487953,
4.4466635296155));
#29938=CARTESIAN_POINT('Ctrl Pts',(13.3681828744984,-0.560257741594785,
3.95454736418435));
#29939=CARTESIAN_POINT('Ctrl Pts',(13.4158987105612,-0.264779785921688,
3.5041710536014));
#29940=CARTESIAN_POINT('Ctrl Pts',(13.4636145466241,0.273849521323983,3.50912209380529));
#29941=CARTESIAN_POINT('Ctrl Pts',(13.5113303826869,0.560998599421335,3.96485386839523));
#29942=CARTESIAN_POINT('Ctrl Pts',(13.5590462187498,0.332974031597074,4.45286087643057));
#29943=CARTESIAN_POINT('Ctrl Pts',(13.6067620548126,-0.200825712906817,
4.52499877347948));
#29944=CARTESIAN_POINT('Ctrl Pts',(13.6544778908754,-0.550204115147588,
4.11502221869768));
#29945=CARTESIAN_POINT('Ctrl Pts',(13.7021937269383,-0.394321612469819,
3.5994189906415));
#29946=CARTESIAN_POINT('Ctrl Pts',(13.7499095630011,0.123672494356884,3.45167546721031));
#29947=CARTESIAN_POINT('Ctrl Pts',(13.7976253990639,0.528096246669736,3.80746679929733));
#29948=CARTESIAN_POINT('Ctrl Pts',(13.8453412351268,0.44756108986054,4.34006433209368));
#29949=CARTESIAN_POINT('Ctrl Pts',(13.8930570711896,-0.0439763023801491,
4.56037555616609));
#29950=CARTESIAN_POINT('Ctrl Pts',(13.9407729072525,-0.495129579482757,
4.26608528452492));
#29951=CARTESIAN_POINT('Ctrl Pts',(13.9884887433153,-0.491597745198497,
3.72744480185615));
#29952=CARTESIAN_POINT('Ctrl Pts',(14.0362045793781,-0.0366241372948624,
3.43909595144367));
#29953=CARTESIAN_POINT('Ctrl Pts',(14.083920415441,0.451981979421435,3.66583391943861));
#29954=CARTESIAN_POINT('Ctrl Pts',(14.1316362515038,0.525526089798339,4.19944174101915));
#29955=CARTESIAN_POINT('Ctrl Pts',(14.1793520875667,0.11647150565515,4.54989914301615));
#29956=CARTESIAN_POINT('Ctrl Pts',(14.2270679236295,-0.399540654275635,
4.39537570069553));
#29957=CARTESIAN_POINT('Ctrl Pts',(14.2747837596924,-0.548648483661927,
3.87777266878906));
#29958=CARTESIAN_POINT('Ctrl Pts',(14.3224995957551,-0.193923968459428,
3.47241287584284));
#29959=CARTESIAN_POINT('Ctrl Pts',(14.370215431818,0.338883910883161,3.5515444569815));
#29960=CARTESIAN_POINT('Ctrl Pts',(14.4179312678808,0.560489480462528,4.04249966364955));
#29961=CARTESIAN_POINT('Ctrl Pts',(14.4656471039437,0.267388935893957,4.49442677524682));
#29962=CARTESIAN_POINT('Ctrl Pts',(14.5133629400065,-0.271258982813659,
4.49231417140114));
#29963=CARTESIAN_POINT('Ctrl Pts',(14.5610787760694,-0.560805603747543,
4.03810188873054));
#29964=CARTESIAN_POINT('Ctrl Pts',(14.6087946121322,-0.335355809656676,
3.54890005536578));
#29965=CARTESIAN_POINT('Ctrl Pts',(14.656510448195,0.198056384554314,3.47395024222346));
#29966=CARTESIAN_POINT('Ctrl Pts',(14.7042262842579,0.549590353339887,3.88208001596329));
#29967=CARTESIAN_POINT('Ctrl Pts',(14.7519421203207,0.396427044118869,4.3984975254762));
#29968=CARTESIAN_POINT('Ctrl Pts',(14.7996579563836,-0.120781319530639,
4.54896862567174));
#29969=CARTESIAN_POINT('Ctrl Pts',(14.8473737924464,-0.527074338995675,
4.19531338994486));
#29970=CARTESIAN_POINT('Ctrl Pts',(14.8950896285092,-0.449346882879826,
3.66229886294881));
#29971=CARTESIAN_POINT('Ctrl Pts',(14.9428054645721,0.041022729875082,3.43940048630678));
#29972=CARTESIAN_POINT('Ctrl Pts',(14.9905213006349,0.493720538569869,3.73130926902151));
#29973=CARTESIAN_POINT('Ctrl Pts',(15.0382371366977,0.493027179828974,4.2699608843321));
#29974=CARTESIAN_POINT('Ctrl Pts',(15.0859529727606,0.0395793756528551,
4.56070326567839));
#29975=CARTESIAN_POINT('Ctrl Pts',(15.1336688088234,-0.450214778192253,
4.33654321062351));
#29976=CARTESIAN_POINT('Ctrl Pts',(15.1813846448863,-0.526569773778615,
3.80333034687015));
#29977=CARTESIAN_POINT('Ctrl Pts',(15.2291004809491,-0.119367643786657,
3.45072225173751));
#29978=CARTESIAN_POINT('Ctrl Pts',(15.2768163170119,0.397451630201876,3.60252436455885));
#29979=CARTESIAN_POINT('Ctrl Pts',(15.3245321530748,0.549284956596614,4.11933446935456));
#29980=CARTESIAN_POINT('Ctrl Pts',(15.3722479891376,0.196701455513243,4.52655789474516));
#29981=CARTESIAN_POINT('Ctrl Pts',(15.4199638252005,-0.336516018808871,
4.45023510325662));
#29982=CARTESIAN_POINT('Ctrl Pts',(15.4676796612633,-0.560705655094284,
3.96045448869));
#29983=CARTESIAN_POINT('Ctrl Pts',(15.5153954973261,-0.269990660741143,
3.50698912564524));
#29984=CARTESIAN_POINT('Ctrl Pts',(15.5631113333889,0.268660911710894,3.50626323446785));
#29985=CARTESIAN_POINT('Ctrl Pts',(15.6108271694518,0.560597035059331,3.95894341219528));
#29986=CARTESIAN_POINT('Ctrl Pts',(15.6585430055146,0.337728275218647,4.44932648624059));
#29987=CARTESIAN_POINT('Ctrl Pts',(15.7062588415775,-0.1952815563728,4.52708613419449));
#29988=CARTESIAN_POINT('Ctrl Pts',(15.7539746776403,-0.548961329954127,
4.12081447485494));
#29989=CARTESIAN_POINT('Ctrl Pts',(15.8016905137031,-0.398521467382777,
3.60359702428645));
#29990=CARTESIAN_POINT('Ctrl Pts',(15.849406349766,0.117886790727162,3.4504025257595));
#29991=CARTESIAN_POINT('Ctrl Pts',(15.8971221858288,0.526037794990907,3.80191184447176));
#29992=CARTESIAN_POINT('Ctrl Pts',(15.9448380218916,0.451120197982628,4.33532856438364));
#29993=CARTESIAN_POINT('Ctrl Pts',(15.9925538579545,-0.0380680182095728,
4.56080790392885));
#29994=CARTESIAN_POINT('Ctrl Pts',(16.0402696940173,-0.492297787528177,
4.27128871615743));
#29995=CARTESIAN_POINT('Ctrl Pts',(16.0879855300802,-0.494442923584513,
3.73264092602517));
#29996=CARTESIAN_POINT('Ctrl Pts',(16.135701366143,-0.0425335149309099,
3.43951308737216));
#29997=CARTESIAN_POINT('Ctrl Pts',(16.1834172022058,0.448435074945997,3.66108900478495));
#29998=CARTESIAN_POINT('Ctrl Pts',(16.2311330382687,0.52759883543946,4.19389210391969));
#29999=CARTESIAN_POINT('Ctrl Pts',(16.2788488743315,0.122260467197297,4.54864110061148));
#30000=CARTESIAN_POINT('Ctrl Pts',(16.3265647103944,-0.395351569291248,
4.39956453268331));
#30001=CARTESIAN_POINT('Ctrl Pts',(16.3742805464572,-0.549906176433804,
3.88356170630145));
#30002=CARTESIAN_POINT('Ctrl Pts',(16.42199638252,-0.199473480363076,3.47448595665642));
#30003=CARTESIAN_POINT('Ctrl Pts',(16.4697122185829,0.334138782019088,3.54799783908671));
#30004=CARTESIAN_POINT('Ctrl Pts',(16.5174280546457,0.560906259487099,4.0365902608309));
#30005=CARTESIAN_POINT('Ctrl Pts',(16.5651438907085,0.272584888215931,4.49158128304055));
#30006=CARTESIAN_POINT('Ctrl Pts',(16.6128597267714,-0.26605538016154,4.49514564908375));
#30007=CARTESIAN_POINT('Ctrl Pts',(16.6605755628342,-0.560372899148451,
4.04401014677825));
#30008=CARTESIAN_POINT('Ctrl Pts',(16.7082913988971,-0.340091362401967,
3.55245944950311));
#30009=CARTESIAN_POINT('Ctrl Pts',(16.7560072349599,0.19250130541649,3.4718921260458));
#30010=CARTESIAN_POINT('Ctrl Pts',(16.8037230710227,0.548317062457662,3.87629438922476));
#30011=CARTESIAN_POINT('Ctrl Pts',(16.8514389070856,0.400604824101502,4.39429741823411));
#30012=CARTESIAN_POINT('Ctrl Pts',(16.8991547431484,-0.114988988324618,
4.55021106103346));
#30013=CARTESIAN_POINT('Ctrl Pts',(16.9468705792113,-0.524986643439221,
4.20085742040038));
#30014=CARTESIAN_POINT('Ctrl Pts',(16.9945864152741,-0.45288098592576,3.66705332002498));
#30015=CARTESIAN_POINT('Ctrl Pts',(17.0423022513369,0.0351122494330066,
3.4389992789138));
#30016=CARTESIAN_POINT('Ctrl Pts',(17.0900180873998,0.490861365866046,3.72612083208173));
#30017=CARTESIAN_POINT('Ctrl Pts',(17.1377339234626,0.49584493715134,4.26474983932169));
#30018=CARTESIAN_POINT('Ctrl Pts',(17.1854497595254,0.0454864730955262,
4.56025499541263));
#30019=CARTESIAN_POINT('Ctrl Pts',(17.2331655955883,-0.446642919103261,
4.34126936858499));
#30020=CARTESIAN_POINT('Ctrl Pts',(17.2808814316511,-0.528613246204851,
3.80889082948154));
#30021=CARTESIAN_POINT('Ctrl Pts',(17.328597267714,-0.125149895556227,3.45201078225777));
#30022=CARTESIAN_POINT('Ctrl Pts',(17.3763131037768,0.393240529860342,3.59835766558462));
#30023=CARTESIAN_POINT('Ctrl Pts',(17.4240289398397,0.55051212592285,4.1135388846668));
#30024=CARTESIAN_POINT('Ctrl Pts',(17.4717447759024,0.202239966032548,4.52445559893916));
#30025=CARTESIAN_POINT('Ctrl Pts',(17.5194606119653,-0.331752266527324,
4.45375666691904));
#30026=CARTESIAN_POINT('Ctrl Pts',(17.5671764480281,-0.561091288070378,
3.96636600572338));
#30027=CARTESIAN_POINT('Ctrl Pts',(17.614892284091,-0.275171546279217,3.50986195899749));
#30028=CARTESIAN_POINT('Ctrl Pts',(17.6626081201538,0.263442460518632,3.50345921706735));
#30029=CARTESIAN_POINT('Ctrl Pts',(17.7103239562167,0.560133202238927,3.95303751636628));
#30030=CARTESIAN_POINT('Ctrl Pts',(17.7580397922795,0.342445005586054,4.44574218699675));
#30031=CARTESIAN_POINT('Ctrl Pts',(17.8057556283423,-0.189715708890181,
4.52911494868296));
#30032=CARTESIAN_POINT('Ctrl Pts',(17.8534714644052,-0.547657568741173,
4.12659331151364));
#30033=CARTESIAN_POINT('Ctrl Pts',(17.901187300468,-0.402677056422281,3.60781908849286));
#30034=CARTESIAN_POINT('Ctrl Pts',(17.9489031365308,0.112087992792125,3.44919063098808));
#30035=CARTESIAN_POINT('Ctrl Pts',(17.9966189725937,0.523920913530056,3.79637889233847));
#30036=CARTESIAN_POINT('Ctrl Pts',(18.0443348086565,0.454629197813879,4.33055554996792));
#30037=CARTESIAN_POINT('Ctrl Pts',(18.0920506447194,-0.0321555056241734,
4.56117795981091));
#30038=CARTESIAN_POINT('Ctrl Pts',(18.1397664807822,-0.489411313471489,
4.27646201432672));
#30039=CARTESIAN_POINT('Ctrl Pts',(18.1874823168451,-0.497233181596917,
3.73786674717144));
#30040=CARTESIAN_POINT('Ctrl Pts',(18.2351981529079,-0.0484381681459794,
3.43999247952716));
#30041=CARTESIAN_POINT('Ctrl Pts',(18.2829139889707,0.444838360430441,3.65638173475637));
#30042=CARTESIAN_POINT('Ctrl Pts',(18.3306298250336,0.529612977905601,4.18832093020544));
#30043=CARTESIAN_POINT('Ctrl Pts',(18.3783456610964,0.128035848626906,4.54732211775687));
#30044=CARTESIAN_POINT('Ctrl Pts',(18.4260614971592,-0.391118570530631,
4.40370898293889));
#30045=CARTESIAN_POINT('Ctrl Pts',(18.4737773332221,-0.551102788237131,
3.88936367722697));
#30046=CARTESIAN_POINT('Ctrl Pts',(18.5214931692849,-0.205000835699102,
3.47661740907615));
#30047=CARTESIAN_POINT('Ctrl Pts',(18.5692090053478,0.329356538604741,3.54450142744705));
#30048=CARTESIAN_POINT('Ctrl Pts',(18.6169248414106,0.561260735706054,4.03067679373969));
#30049=CARTESIAN_POINT('Ctrl Pts',(18.6646406774734,0.2777505631021,4.48868118831814));
#30050=CARTESIAN_POINT('Ctrl Pts',(18.7123565135363,-0.260822225340423,
4.49792212833724));
#30051=CARTESIAN_POINT('Ctrl Pts',(18.7600723495991,-0.559877950986752,
4.04991351638789));
#30052=CARTESIAN_POINT('Ctrl Pts',(18.8077881856619,-0.344789139412875,
3.55606855432066));
#30053=CARTESIAN_POINT('Ctrl Pts',(18.8555040217248,0.186924844147682,3.46989266958543));
#30054=CARTESIAN_POINT('Ctrl Pts',(18.9032198577876,0.546982867117114,3.87052250311704));
#30055=CARTESIAN_POINT('Ctrl Pts',(18.9509356938504,0.404738106803207,4.39005351430856));
#30056=CARTESIAN_POINT('Ctrl Pts',(18.9986515299133,-0.109183884691052,
4.55139238155646));
#30057=CARTESIAN_POINT('Ctrl Pts',(19.0463673659761,-0.522840634850846,
4.20637914057629));
#30058=CARTESIAN_POINT('Ctrl Pts',(19.094083202039,-0.456364785113784,3.67184475922049));
#30059=CARTESIAN_POINT('Ctrl Pts',(19.1417990381018,0.029197868913272,3.43866038485254));
#30060=CARTESIAN_POINT('Ctrl Pts',(19.1895148741647,0.487947670564988,3.72096281627648));
#30061=CARTESIAN_POINT('Ctrl Pts',(19.2372307102275,0.498607618457993,4.25950938727589));
#30062=CARTESIAN_POINT('Ctrl Pts',(19.2849465462903,0.0513885179525073,
4.55974449445321));
#30063=CARTESIAN_POINT('Ctrl Pts',(19.3326623823531,-0.44302144872845,4.34595762039384));
#30064=CARTESIAN_POINT('Ctrl Pts',(19.380378218416,-0.530598003365269,3.81447253878192));
#30065=CARTESIAN_POINT('Ctrl Pts',(19.4280940544788,-0.130918245164485,
3.45336018235082));
#30066=CARTESIAN_POINT('Ctrl Pts',(19.4758098905417,0.38898574814073,3.59423557624425));
#30067=CARTESIAN_POINT('Ctrl Pts',(19.5235257266045,0.551678150913516,4.10773069407674));
#30068=CARTESIAN_POINT('Ctrl Pts',(19.5712415626673,0.207756005258534,4.52229503878775));
#30069=CARTESIAN_POINT('Ctrl Pts',(19.6189573987302,-0.326951650734615,
4.4572278489044));
#30070=CARTESIAN_POINT('Ctrl Pts',(19.666673234793,-0.561414624206118,3.9722812219163));
#30071=CARTESIAN_POINT('Ctrl Pts',(19.7143890708559,-0.280321816997631,
3.51278930393937));
#30072=CARTESIAN_POINT('Ctrl Pts',(19.7621049069187,0.258194652845487,3.5007102220535));
#30073=CARTESIAN_POINT('Ctrl Pts',(19.8098207429815,0.559607330995945,3.94713708427543));
#30074=CARTESIAN_POINT('Ctrl Pts',(19.8575365790444,0.347123361713752,4.44210790974427));
#30075=CARTESIAN_POINT('Ctrl Pts',(19.9052524151072,-0.184128152223511,
4.53108587353909));
#30076=CARTESIAN_POINT('Ctrl Pts',(19.9529682511701,-0.546294178096705,
4.13235642149579));
#30077=CARTESIAN_POINT('Ctrl Pts',(20.0006840872329,-0.406785648814185,
3.61208785870539));
#30078=CARTESIAN_POINT('Ctrl Pts',(20.0483999232957,0.106272459957556,3.44803398021027));
#30079=CARTESIAN_POINT('Ctrl Pts',(20.0961157593586,0.5217539278249,3.7908797683689));
#30080=CARTESIAN_POINT('Ctrl Pts',(20.1438315954214,0.458072423058868,4.32572464996293));
#30081=CARTESIAN_POINT('Ctrl Pts',(20.1915474314842,-0.0262105744965466,
4.56152565902554));
#30082=CARTESIAN_POINT('Ctrl Pts',(20.2392632675471,-0.486524960252488,
4.28152908133109));
#30083=CARTESIAN_POINT('Ctrl Pts',(20.2869791036099,-0.499865224545849,
3.74326461201656));
#30084=CARTESIAN_POINT('Ctrl Pts',(20.3346949396728,-0.0545328049175168,
3.440261547834));
#30085=CARTESIAN_POINT('Ctrl Pts',(20.3824107757356,0.441568512678419,3.6522489094147));
#30086=CARTESIAN_POINT('Ctrl Pts',(20.4221739724547,0.515928418030698,4.09332268501583));
#30087=CARTESIAN_POINT('Ctrl Pts',(20.4539845298298,0.333108474939506,4.36566768059473));
#30088=CARTESIAN_POINT('Ctrl Pts',(20.4778424478613,0.118510552090848,4.48142006140068));
#30089=CARTESIAN_POINT('Ctrl Pts',(20.5017003658927,-0.127372553428812,
4.47887124859312));
#30090=CARTESIAN_POINT('Ctrl Pts',(20.5255582839241,-0.340862259689409,
4.35954554232165));
#30091=CARTESIAN_POINT('Ctrl Pts',(20.5494162019555,-0.471665647836603,
4.15213005589169));
#30092=CARTESIAN_POINT('Ctrl Pts',(20.5732741199869,-0.486782001098211,
3.90760543082941));
#30093=CARTESIAN_POINT('Ctrl Pts',(20.5971320380184,-0.38305332993788,3.68562568155832));
#30094=CARTESIAN_POINT('Ctrl Pts',(20.6209899560498,-0.185558943137764,
3.54054450025879));
#30095=CARTESIAN_POINT('Ctrl Pts',(20.6448478740812,0.0572573647513246,
3.50779920733485));
#30096=CARTESIAN_POINT('Ctrl Pts',(20.6687057921126,0.28610038304352,3.59541756340761));
#30097=CARTESIAN_POINT('Ctrl Pts',(20.6925637101441,0.444969396676924,3.78196356026503));
#30098=CARTESIAN_POINT('Ctrl Pts',(20.7164216281754,0.495039040219165,4.02182741068269));
#30099=CARTESIAN_POINT('Ctrl Pts',(20.7402795462069,0.424054039808096,4.25635280284423));
#30100=CARTESIAN_POINT('Ctrl Pts',(20.7641374642383,0.249378454468877,4.42819351412177));
#30101=CARTESIAN_POINT('Ctrl Pts',(20.7879953822697,0.0137218901755031,
4.49532894963167));
#30102=CARTESIAN_POINT('Ctrl Pts',(20.8118533003011,-0.22528943893053,4.44134312218709));
#30103=CARTESIAN_POINT('Ctrl Pts',(20.8357112183326,-0.409211687104306,
4.27943679589328));
#30104=CARTESIAN_POINT('Ctrl Pts',(20.859569136364,-0.493070359673604,4.04920060553547));
#30105=CARTESIAN_POINT('Ctrl Pts',(20.8834270543954,-0.456359989112496,
3.80693350349834));
#30106=CARTESIAN_POINT('Ctrl Pts',(20.9072849724268,-0.308057122141145,
3.61187643128937));
#30107=CARTESIAN_POINT('Ctrl Pts',(20.9311428904583,-0.0844259229598539,
3.51172613733272));
#30108=CARTESIAN_POINT('Ctrl Pts',(20.9550008084896,0.159849727585384,3.53097210659131));
#30109=CARTESIAN_POINT('Ctrl Pts',(20.9788587265211,0.365037758375503,3.66490817000854));
#30110=CARTESIAN_POINT('Ctrl Pts',(21.0027166445525,0.480964117596,3.88078331455297));
#30111=CARTESIAN_POINT('Ctrl Pts',(21.026574562584,0.479281646861755,4.12581018556955));
#30112=CARTESIAN_POINT('Ctrl Pts',(21.0504324806153,0.360401759160676,4.34007303948752));
#30113=CARTESIAN_POINT('Ctrl Pts',(21.0742903986468,0.153393823636192,4.47117877170218));
#30114=CARTESIAN_POINT('Ctrl Pts',(21.0981483166782,-0.0911230798336762,
4.48706845966041));
#30115=CARTESIAN_POINT('Ctrl Pts',(21.1220062347096,-0.313357908298923,
4.38385664171252));
#30116=CARTESIAN_POINT('Ctrl Pts',(21.145864152741,-0.458968192403581,4.18678141884249));
#30117=CARTESIAN_POINT('Ctrl Pts',(21.1697220707724,-0.492348251467217,
3.94403305123036));
#30118=CARTESIAN_POINT('Ctrl Pts',(21.1935799888039,-0.405335751726616,
3.71497012710753));
#30119=CARTESIAN_POINT('Ctrl Pts',(21.2174379068353,-0.21920761957706,3.55560477096155));
#30120=CARTESIAN_POINT('Ctrl Pts',(21.2412958248667,0.0205227466613194,
3.50490615340017));
#30121=CARTESIAN_POINT('Ctrl Pts',(21.2651537428981,0.255234742309135,3.57527146741714));
#30122=CARTESIAN_POINT('Ctrl Pts',(21.2890116609295,0.427534891009427,3.74949447702405));
#30123=CARTESIAN_POINT('Ctrl Pts',(21.312869578961,0.495291113040325,3.98497291063177));
#30124=CARTESIAN_POINT('Ctrl Pts',(21.3367274969923,0.441935166474334,4.22412587691986));
#30125=CARTESIAN_POINT('Ctrl Pts',(21.3605854150238,0.280514033632862,4.40847396123464));
#30126=CARTESIAN_POINT('Ctrl Pts',(21.3844433330552,0.0504995785194436,
4.49293903542029));
#30127=CARTESIAN_POINT('Ctrl Pts',(21.4083012510867,-0.191863399122956,
4.45686708805594));
#30128=CARTESIAN_POINT('Ctrl Pts',(21.432159169118,-0.387310549425693,4.3090786928523));
#30129=CARTESIAN_POINT('Ctrl Pts',(21.4560170871495,-0.488049720266331,
4.08571213811173));
#30130=CARTESIAN_POINT('Ctrl Pts',(21.4798750051809,-0.469447440294381,
3.84138663085107));
#30131=CARTESIAN_POINT('Ctrl Pts',(21.5037329232123,-0.336052473678932,
3.63584641288874));
#30132=CARTESIAN_POINT('Ctrl Pts',(21.5275908412437,-0.120483523363382,
3.51935166631968));
#30133=CARTESIAN_POINT('Ctrl Pts',(21.5514487592752,0.124546930319796,3.5203885299332));
#30134=CARTESIAN_POINT('Ctrl Pts',(21.5753066773065,0.339122266949511,3.63870346233219));
#30135=CARTESIAN_POINT('Ctrl Pts',(21.599164595338,0.470772971804989,3.84536523971104));
#30136=CARTESIAN_POINT('Ctrl Pts',(21.6230225133694,0.487306861455871,4.08983942814686));
#30137=CARTESIAN_POINT('Ctrl Pts',(21.6468804314008,0.384680949508402,4.31234542922385));
#30138=CARTESIAN_POINT('Ctrl Pts',(21.6707383494323,0.187990066907445,4.45847446473699));
#30139=CARTESIAN_POINT('Ctrl Pts',(21.6945962674636,-0.0546695077989956,
4.49249400502822));
#30140=CARTESIAN_POINT('Ctrl Pts',(21.7184541854951,-0.283960898681086,
4.40608534582272));
#30141=CARTESIAN_POINT('Ctrl Pts',(21.7423121035264,-0.443816114896065,
4.22037775802082));
#30142=CARTESIAN_POINT('Ctrl Pts',(21.766170021558,-0.495146201710716,3.98078180541326));
#30143=CARTESIAN_POINT('Ctrl Pts',(21.7900279395893,-0.425399554695369,
3.74588522487523));
#30144=CARTESIAN_POINT('Ctrl Pts',(21.8138858576208,-0.25163112890579,3.57312662880273));
#30145=CARTESIAN_POINT('Ctrl Pts',(21.8377437756521,-0.0163320378044167,
3.50475019978512));
#30146=CARTESIAN_POINT('Ctrl Pts',(21.8616016936836,0.222960681415914,3.55747583725374));
#30147=CARTESIAN_POINT('Ctrl Pts',(21.885459611715,0.407733440703041,3.71841068663001));
#30148=CARTESIAN_POINT('Ctrl Pts',(21.9093175297464,0.492804267302335,3.94820179346412));
#30149=CARTESIAN_POINT('Ctrl Pts',(21.9331754477779,0.457371026827486,4.19065897275109));
#30150=CARTESIAN_POINT('Ctrl Pts',(21.9570333658092,0.310098111756678,4.38649483975425));
#30151=CARTESIAN_POINT('Ctrl Pts',(21.9808912838407,0.0869977614584207,
4.48782219052945));
#30152=CARTESIAN_POINT('Ctrl Pts',(22.0047492018721,-0.15737591128791,4.46986372771052));
#30153=CARTESIAN_POINT('Ctrl Pts',(22.0286071199035,-0.363266886890503,
4.33701078463543));
#30154=CARTESIAN_POINT('Ctrl Pts',(22.0524650379349,-0.480329213457224,
4.12174952472744));
#30155=CARTESIAN_POINT('Ctrl Pts',(22.0763229559664,-0.479937963428243,
3.87671718963328));
#30156=CARTESIAN_POINT('Ctrl Pts',(22.1001808739978,-0.362188808094022,
3.66183085982978));
#30157=CARTESIAN_POINT('Ctrl Pts',(22.1240387920292,-0.155874623354616,
3.529636096341));
#30158=CARTESIAN_POINT('Ctrl Pts',(22.1478967100606,0.0885551527323001,
3.51245811975107));
#30159=CARTESIAN_POINT('Ctrl Pts',(22.1717546280921,0.311330781786364,3.61449741325855));
#30160=CARTESIAN_POINT('Ctrl Pts',(22.1956125461234,0.457977554205651,3.81080259009947));
#30161=CARTESIAN_POINT('Ctrl Pts',(22.2194704641549,0.492636339578261,4.05337168730347));
#30162=CARTESIAN_POINT('Ctrl Pts',(22.2433283821863,0.406832120751761,4.28288995313029));
#30163=CARTESIAN_POINT('Ctrl Pts',(22.2671863002177,0.22154636656941,4.44323391967918));
#30164=CARTESIAN_POINT('Ctrl Pts',(22.2910442182491,-0.0179135091400202,
4.49519511936025));
#30165=CARTESIAN_POINT('Ctrl Pts',(22.3149021362805,-0.2529930437236,4.42606762362056));
#30166=CARTESIAN_POINT('Ctrl Pts',(22.338760054312,-0.426208888077552,4.25275498785448));
#30167=CARTESIAN_POINT('Ctrl Pts',(22.3626179723434,-0.495205048933098,
4.01763687303198));
#30168=CARTESIAN_POINT('Ctrl Pts',(22.3864758903748,-0.443110087468167,
3.77820606161377));
#30169=CARTESIAN_POINT('Ctrl Pts',(22.4103338084062,-0.282662637164788,
3.59300991103726));
#30170=CARTESIAN_POINT('Ctrl Pts',(22.4341917264377,-0.0530964769854286,
3.50733392083031));
#30171=CARTESIAN_POINT('Ctrl Pts',(22.458049644469,0.189453226607198,3.5421282117862));
#30172=CARTESIAN_POINT('Ctrl Pts',(22.4819075625005,0.385676439696491,3.6888846179772));
#30173=CARTESIAN_POINT('Ctrl Pts',(22.5057654805319,0.487591287867653,3.9117172269821));
#30174=CARTESIAN_POINT('Ctrl Pts',(22.5296233985634,0.470276727405835,4.15613734610506));
#30175=CARTESIAN_POINT('Ctrl Pts',(22.5534813165947,0.337966804695391,4.36237769267677));
#30176=CARTESIAN_POINT('Ctrl Pts',(22.5773392346262,0.123014588878675,4.48000670597833));
#30177=CARTESIAN_POINT('Ctrl Pts',(22.6011971526576,-0.122017660845505,
4.48026122441149));
#30178=CARTESIAN_POINT('Ctrl Pts',(22.625055070689,-0.337213993725473,4.36307837627545));
#30179=CARTESIAN_POINT('Ctrl Pts',(22.6489129887204,-0.469950950795418,
4.15711375897153));
#30180=CARTESIAN_POINT('Ctrl Pts',(22.6727709067518,-0.487774683880463,
3.912729067726));
#30181=CARTESIAN_POINT('Ctrl Pts',(22.6966288247832,-0.386319338946922,
3.6896872918462));
#30182=CARTESIAN_POINT('Ctrl Pts',(22.7204867428147,-0.190407614498503,
3.54252014522276));
#30183=CARTESIAN_POINT('Ctrl Pts',(22.7443446608461,0.0520814161336476,
3.50722927763546));
#30184=CARTESIAN_POINT('Ctrl Pts',(22.7682025788775,0.281801791424649,3.59241522467272));
#30185=CARTESIAN_POINT('Ctrl Pts',(22.7920604969089,0.442679857002608,3.77730419914427));
#30186=CARTESIAN_POINT('Ctrl Pts',(22.8079657755965,0.477669651496365,3.93681187972983));
#30187=CARTESIAN_POINT('Ctrl Pts',(22.8159184149403,0.475016281724327,4.01593044384941));
#30188=CARTESIAN_POINT('Ctrl Pts',(3.98408158505964,0.229225853138217,4.48306385360099));
#30189=CARTESIAN_POINT('Ctrl Pts',(3.99203422440344,0.148766887950233,4.52124364039387));
#30190=CARTESIAN_POINT('Ctrl Pts',(4.00793950309106,-0.0315132651739855,
4.55658776856145));
#30191=CARTESIAN_POINT('Ctrl Pts',(4.03179742112247,-0.29437836981663,4.47338935048851));
#30192=CARTESIAN_POINT('Ctrl Pts',(4.0556553391539,-0.485191777607318,4.27448557757091));
#30193=CARTESIAN_POINT('Ctrl Pts',(4.07951325718531,-0.557397168683185,
4.00843674174317));
#30194=CARTESIAN_POINT('Ctrl Pts',(4.10337117521674,-0.493285636019562,
3.74033843218029));
#30195=CARTESIAN_POINT('Ctrl Pts',(4.12722909324815,-0.308561908987092,
3.53572729771651));
#30196=CARTESIAN_POINT('Ctrl Pts',(4.15108701127957,-0.0483813190761145,
3.44464727048097));
#30197=CARTESIAN_POINT('Ctrl Pts',(4.17494492931099,0.223627135909104,3.48936410886239));
#30198=CARTESIAN_POINT('Ctrl Pts',(4.19880284734241,0.440954086798485,3.65894639349553));
#30199=CARTESIAN_POINT('Ctrl Pts',(4.22266076537383,0.55045499896491,3.91192501290154));
#30200=CARTESIAN_POINT('Ctrl Pts',(4.24651868340524,0.525355068663259,4.18644066347397));
#30201=CARTESIAN_POINT('Ctrl Pts',(4.27037660143667,0.371791302444591,4.41536633561891));
#30202=CARTESIAN_POINT('Ctrl Pts',(4.29423451946808,0.127314547262185,4.54272370785395));
#30203=CARTESIAN_POINT('Ctrl Pts',(4.31809243749951,-0.14829414195428,4.5373703057994));
#30204=CARTESIAN_POINT('Ctrl Pts',(4.34195035553092,-0.387640842632661,
4.40061524972397));
#30205=CARTESIAN_POINT('Ctrl Pts',(4.36580827356235,-0.53219881478122,4.16589884014724));
#30206=CARTESIAN_POINT('Ctrl Pts',(4.38966619159376,-0.546619671109945,
3.89061565172978));
#30207=CARTESIAN_POINT('Ctrl Pts',(4.41352410962518,-0.427377132892538,
3.64207991255526));
#30208=CARTESIAN_POINT('Ctrl Pts',(4.4373820276566,-0.203629241694984,3.48106538615089));
#30209=CARTESIAN_POINT('Ctrl Pts',(4.46123994568802,0.0699115445388116,
3.44694450735191));
#30210=CARTESIAN_POINT('Ctrl Pts',(4.48509786371944,0.326357054473012,3.54806076195131));
#30211=CARTESIAN_POINT('Ctrl Pts',(4.50895578175085,0.502999374434197,3.7596884705576));
#30212=CARTESIAN_POINT('Ctrl Pts',(4.53281369978229,0.556644646112557,4.03007889421215));
#30213=CARTESIAN_POINT('Ctrl Pts',(4.55667161781369,0.474175139017821,4.29311420882242));
#30214=CARTESIAN_POINT('Ctrl Pts',(4.58052953584512,0.275756894216243,4.48447511514554));
#30215=CARTESIAN_POINT('Ctrl Pts',(4.60438745387653,0.00990857728296194,
4.55736865895685));
#30216=CARTESIAN_POINT('Ctrl Pts',(4.62824537190795,-0.258362656684952,
4.49397038324719));
#30217=CARTESIAN_POINT('Ctrl Pts',(4.65210328993938,-0.463457183444019,
4.30978289334447));
#30218=CARTESIAN_POINT('Ctrl Pts',(4.67596120797079,-0.555223804526532,
4.04984504770563));
#30219=CARTESIAN_POINT('Ctrl Pts',(4.69981912600221,-0.511223081411799,
3.77771873014923));
#30220=CARTESIAN_POINT('Ctrl Pts',(4.72367704403363,-0.342214389453536,
3.55994623789246));
#30221=CARTESIAN_POINT('Ctrl Pts',(4.74753496206505,-0.0895249575417115,
3.44977887729433));
#30222=CARTESIAN_POINT('Ctrl Pts',(4.77139288009647,0.185055765100279,3.47415556892044));
#30223=CARTESIAN_POINT('Ctrl Pts',(4.79525079812788,0.414385312357242,3.62711554766008));
#30224=CARTESIAN_POINT('Ctrl Pts',(4.81910871615931,0.542386363113676,3.87125593216545));
#30225=CARTESIAN_POINT('Ctrl Pts',(4.84296663419071,0.537759173780872,4.14687774817434));
#30226=CARTESIAN_POINT('Ctrl Pts',(4.86682455222215,0.401635218192884,4.38658395388507));
#30227=CARTESIAN_POINT('Ctrl Pts',(4.89068247025356,0.167300511433038,4.53175985253543));
#30228=CARTESIAN_POINT('Ctrl Pts',(4.91454038828499,-0.107943727546613,
4.54690598239331));
#30229=CARTESIAN_POINT('Ctrl Pts',(4.9383983063164,-0.356792784813018,4.42831870213619));
#30230=CARTESIAN_POINT('Ctrl Pts',(4.96225622434782,-0.518396287352312,
4.20499583203957));
#30231=CARTESIAN_POINT('Ctrl Pts',(4.98611414237924,-0.553237776802617,
3.93154589703492));
#30232=CARTESIAN_POINT('Ctrl Pts',(5.00997206041066,-0.452797559930213,
3.67483485485756));
#30233=CARTESIAN_POINT('Ctrl Pts',(5.03382997844208,-0.241636005696979,
3.49763554798826));
#30234=CARTESIAN_POINT('Ctrl Pts',(5.05768789647349,0.0286121339618079,
3.44327803376872));
#30235=CARTESIAN_POINT('Ctrl Pts',(5.08154581450492,0.291863827488053,3.52505420509465));
#30236=CARTESIAN_POINT('Ctrl Pts',(5.10540373253633,0.48374686498243,3.72296756053861));
#30237=CARTESIAN_POINT('Ctrl Pts',(5.12926165056775,0.557340616988569,3.98862289364304));
#30238=CARTESIAN_POINT('Ctrl Pts',(5.15311956859917,0.49464940648741,4.25706023915787));
#30239=CARTESIAN_POINT('Ctrl Pts',(5.17697748663059,0.311002942120779,4.46263935401832));
#30240=CARTESIAN_POINT('Ctrl Pts',(5.20083540466201,0.0513077868555636,
4.55509054477827));
#30241=CARTESIAN_POINT('Ctrl Pts',(5.22469332269342,-0.22093351989189,4.5118069769771));
#30242=CARTESIAN_POINT('Ctrl Pts',(5.24855124072485,-0.439150562917527,
4.34337266196288));
#30243=CARTESIAN_POINT('Ctrl Pts',(5.27240915875626,-0.549983331088669,
4.09097437781523));
#30244=CARTESIAN_POINT('Ctrl Pts',(5.29626707678769,-0.526330193563486,
3.81633038019944));
#30245=CARTESIAN_POINT('Ctrl Pts',(5.32012499481911,-0.373974986765411,
3.5865986076849));
#30246=CARTESIAN_POINT('Ctrl Pts',(5.34398291285052,-0.130172708829089,
3.45795473641922));
#30247=CARTESIAN_POINT('Ctrl Pts',(5.36784083088195,0.145460342249349,3.46185569711558));
#30248=CARTESIAN_POINT('Ctrl Pts',(5.39169874891335,0.385524377387638,3.59734759862366));
#30249=CARTESIAN_POINT('Ctrl Pts',(5.41555666694479,0.531317200781484,3.83129898029949));
#30250=CARTESIAN_POINT('Ctrl Pts',(5.4394145849762,0.547188495794237,4.10650235661553));
#30251=CARTESIAN_POINT('Ctrl Pts',(5.46327250300762,0.42925729847004,4.35566300567327));
#30252=CARTESIAN_POINT('Ctrl Pts',(5.48713042103904,0.206360998935678,4.51785436177788));
#30253=CARTESIAN_POINT('Ctrl Pts',(5.51098833907045,-0.0669961859988386,
4.55341622035867));
#30254=CARTESIAN_POINT('Ctrl Pts',(5.53484625710188,-0.323970978517869,
4.45365273830571));
#30255=CARTESIAN_POINT('Ctrl Pts',(5.55870417513329,-0.501726041995696,
4.2429588044862));
#30256=CARTESIAN_POINT('Ctrl Pts',(5.58256209316472,-0.556795421465071,
3.97285482490167));
#30257=CARTESIAN_POINT('Ctrl Pts',(5.60642001119613,-0.475713153578786,
3.70938858005442));
#30258=CARTESIAN_POINT('Ctrl Pts',(5.63027792922756,-0.27830606148521,3.51698474346866));
#30259=CARTESIAN_POINT('Ctrl Pts',(5.65413584725897,-0.0128455564368745,
3.44269129419766));
#30260=CARTESIAN_POINT('Ctrl Pts',(5.67799376529039,0.255756037034639,3.5046750042392));
#30261=CARTESIAN_POINT('Ctrl Pts',(5.70185168332181,0.46181831285622,3.68777916820271));
#30262=CARTESIAN_POINT('Ctrl Pts',(5.72570960135323,0.554953431393631,3.94722983012095));
#30263=CARTESIAN_POINT('Ctrl Pts',(5.74956751938465,0.512387319539865,4.21958423627784));
#30264=CARTESIAN_POINT('Ctrl Pts',(5.77342543741606,0.344528550506956,4.43824431479549));
#30265=CARTESIAN_POINT('Ctrl Pts',(5.79728335544749,0.0924231668635294,
4.54974172178225));
#30266=CARTESIAN_POINT('Ctrl Pts',(5.82114127347891,-0.182282200065281,
4.52681230129395));
#30267=CARTESIAN_POINT('Ctrl Pts',(5.84499919151032,-0.412414601109181,
4.37506292652603));
#30268=CARTESIAN_POINT('Ctrl Pts',(5.86885710954175,-0.541700403334708,
4.13160044316952));
#30269=CARTESIAN_POINT('Ctrl Pts',(5.89271502757316,-0.538525691690445,
3.85595807909033));
#30270=CARTESIAN_POINT('Ctrl Pts',(5.91657294560459,-0.403666797469215,
3.61553786496538));
#30271=CARTESIAN_POINT('Ctrl Pts',(5.94043086363599,-0.170100341263849,
3.46912915944898));
#30272=CARTESIAN_POINT('Ctrl Pts',(5.96428878166742,0.105060216979666,3.45253275189516));
#30273=CARTESIAN_POINT('Ctrl Pts',(5.98814669969884,0.354530812822036,3.5698071562788));
#30274=CARTESIAN_POINT('Ctrl Pts',(6.01200461773026,0.517308736525128,3.79227513259484));
#30275=CARTESIAN_POINT('Ctrl Pts',(6.03586253576167,0.553591019453439,4.06553805729756));
#30276=CARTESIAN_POINT('Ctrl Pts',(6.0597204537931,0.454504394384077,4.32277408438697));
#30277=CARTESIAN_POINT('Ctrl Pts',(6.08357837182452,0.244280620740535,4.50108505220882));
#30278=CARTESIAN_POINT('Ctrl Pts',(6.10743628985593,-0.0256793573627324,
4.55686330558177));
#30279=CARTESIAN_POINT('Ctrl Pts',(6.13129420788736,-0.289354484390735,
4.47648043042773));
#30280=CARTESIAN_POINT('Ctrl Pts',(6.15515212591877,-0.482285035214929,
4.27957167009689));
#30281=CARTESIAN_POINT('Ctrl Pts',(6.17901004395019,-0.557263974895364,
4.01432540012922));
#30282=CARTESIAN_POINT('Ctrl Pts',(6.20286796198161,-0.496014047041978,
3.74552825888183));
#30283=CARTESIAN_POINT('Ctrl Pts',(6.22672588001303,-0.313404643062,3.53904687299508));
#30284=CARTESIAN_POINT('Ctrl Pts',(6.25058379804445,-0.0542924323345977,
3.44511024149985));
#30285=CARTESIAN_POINT('Ctrl Pts',(6.27444171607587,0.218347115212216,3.48718178027374));
#30286=CARTESIAN_POINT('Ctrl Pts',(6.29829963410728,0.437120926894882,3.65404298137615));
#30287=CARTESIAN_POINT('Ctrl Pts',(6.32215755213871,0.549895923261456,3.90664388593688));
#30288=CARTESIAN_POINT('Ctrl Pts',(6.34601547017011,0.526573903738089,4.17995327069166));
#30289=CARTESIAN_POINT('Ctrl Pts',(6.37782602754536,0.327418726170013,4.4906154426808));
#30290=CARTESIAN_POINT('Ctrl Pts',(6.41758922426438,-0.161063729547888,
4.61146011675295));
#30291=CARTESIAN_POINT('Ctrl Pts',(6.46530506032721,-0.60205854017139,4.19446204504257));
#30292=CARTESIAN_POINT('Ctrl Pts',(6.51302089639007,-0.488859252747234,
3.59916283817905));
#30293=CARTESIAN_POINT('Ctrl Pts',(6.56073673245289,0.0725864685289804,
3.37181094029106));
#30294=CARTESIAN_POINT('Ctrl Pts',(6.60845256851574,0.567733426150434,3.72141305678318));
#30295=CARTESIAN_POINT('Ctrl Pts',(6.65616840457857,0.541332409494817,4.32680434473755));
#30296=CARTESIAN_POINT('Ctrl Pts',(6.70388424064141,0.0179179137367747,
4.6321081579338));
#30297=CARTESIAN_POINT('Ctrl Pts',(6.75160007670425,-0.522004047715759,
4.35692568061372));
#30298=CARTESIAN_POINT('Ctrl Pts',(6.79931591276708,-0.582533501572452,
3.75397902491298));
#30299=CARTESIAN_POINT('Ctrl Pts',(6.84703174882993,-0.10812839031349,3.37695395054049));
#30300=CARTESIAN_POINT('Ctrl Pts',(6.89474758489276,0.465580583415614,3.57208337966475));
#30301=CARTESIAN_POINT('Ctrl Pts',(6.9424634209556,0.611735560770294,4.16017430964564));
#30302=CARTESIAN_POINT('Ctrl Pts',(6.99017925701844,0.196126575106773,4.60117519156627));
#30303=CARTESIAN_POINT('Ctrl Pts',(7.03789509308127,-0.399589635450545,
4.49010738789885));
#30304=CARTESIAN_POINT('Ctrl Pts',(7.08561092914412,-0.628355913977057,
3.92896656470948));
#30305=CARTESIAN_POINT('Ctrl Pts',(7.13332676520695,-0.280093617253323,
3.43305676608093));
#30306=CARTESIAN_POINT('Ctrl Pts',(7.1810426012698,0.325383132256395,3.45777970086456));
#30307=CARTESIAN_POINT('Ctrl Pts',(7.22875843733263,0.632055452459012,3.98043185926557));
#30308=CARTESIAN_POINT('Ctrl Pts',(7.27647427339546,0.358301574124045,4.52105375310108));
#30309=CARTESIAN_POINT('Ctrl Pts',(7.32419010945831,-0.244486178793781,
4.58318396235269));
#30310=CARTESIAN_POINT('Ctrl Pts',(7.37190594552114,-0.622758498112341,
4.10976736853928));
#30311=CARTESIAN_POINT('Ctrl Pts',(7.41962178158399,-0.42914211350377,3.53554970961824));
#30312=CARTESIAN_POINT('Ctrl Pts',(7.46733761764681,0.158562080980748,3.38784389968312));
#30313=CARTESIAN_POINT('Ctrl Pts',(7.51505345370967,0.600656274672958,3.80229045545538));
#30314=CARTESIAN_POINT('Ctrl Pts',(7.56276928977248,0.491158570126743,4.3982967283715));
#30315=CARTESIAN_POINT('Ctrl Pts',(7.61048512583535,-0.0693776073840611,
4.62854098691609));
#30316=CARTESIAN_POINT('Ctrl Pts',(7.65820096189817,-0.566203260219877,
4.28158638589565));
#30317=CARTESIAN_POINT('Ctrl Pts',(7.70591679796101,-0.543075747198986,
3.67604667390869));
#30318=CARTESIAN_POINT('Ctrl Pts',(7.75363263402386,-0.0212334191459514,
3.36799828595259));
#30319=CARTESIAN_POINT('Ctrl Pts',(7.80134847008666,0.520107884382028,3.64032679659274));
#30320=CARTESIAN_POINT('Ctrl Pts',(7.84906430614954,0.583826114817312,4.24294874421058));
#30321=CARTESIAN_POINT('Ctrl Pts',(7.89678014221235,0.111407840683781,4.62246712177016));
#30322=CARTESIAN_POINT('Ctrl Pts',(7.94449597827521,-0.463317967772962,
4.43036436352186));
#30323=CARTESIAN_POINT('Ctrl Pts',(7.99221181433803,-0.612571757364041,
3.84305138824375));
#30324=CARTESIAN_POINT('Ctrl Pts',(8.03992765040088,-0.199291476537812,
3.39986673810663));
#30325=CARTESIAN_POINT('Ctrl Pts',(8.08764348646372,0.397001233685627,3.50779369660314));
#30326=CARTESIAN_POINT('Ctrl Pts',(8.13535932252656,0.628721602366905,4.06772127707659));
#30327=CARTESIAN_POINT('Ctrl Pts',(8.18307515858938,0.283077249469033,4.56545936678474));
#30328=CARTESIAN_POINT('Ctrl Pts',(8.23079099465223,-0.32252129731946,4.54392741926377));
#30329=CARTESIAN_POINT('Ctrl Pts',(8.27850683071506,-0.631943574151527,
4.02289855323374));
#30330=CARTESIAN_POINT('Ctrl Pts',(8.32622266677791,-0.361042343138453,
3.48084159342964));
#30331=CARTESIAN_POINT('Ctrl Pts',(8.37393850284074,0.241409626929164,3.41553578665797));
#30332=CARTESIAN_POINT('Ctrl Pts',(8.42165433890358,0.622171422023167,3.88695246013618));
#30333=CARTESIAN_POINT('Ctrl Pts',(8.46937017496642,0.431583626935426,4.46218242893131));
#30334=CARTESIAN_POINT('Ctrl Pts',(8.51708601102927,-0.155334053534803,
4.61298316164806));
#30335=CARTESIAN_POINT('Ctrl Pts',(8.56480184709209,-0.599606082522386,
4.20087202506506));
#30336=CARTESIAN_POINT('Ctrl Pts',(8.61251768315494,-0.493250619804184,
3.60429701705146));
#30337=CARTESIAN_POINT('Ctrl Pts',(8.66023351921777,0.0660644767165412,
3.37110214695249));
#30338=CARTESIAN_POINT('Ctrl Pts',(8.70794935528061,0.564711547735832,3.71543385214437));
#30339=CARTESIAN_POINT('Ctrl Pts',(8.75566519134344,0.544775315265253,4.32108702952508));
#30340=CARTESIAN_POINT('Ctrl Pts',(8.80338102740629,0.0245635283409047,
4.6318810471339));
#30341=CARTESIAN_POINT('Ctrl Pts',(8.85109686346912,-0.518205324617361,
4.36240897642002));
#30342=CARTESIAN_POINT('Ctrl Pts',(8.89881269953197,-0.585098254365674,
3.76013116628075));
#30343=CARTESIAN_POINT('Ctrl Pts',(8.9465285355948,-0.114686454236133,3.3781285970023));
#30344=CARTESIAN_POINT('Ctrl Pts',(8.99424437165764,0.461043681496376,3.56720010581811));
#30345=CARTESIAN_POINT('Ctrl Pts',(9.04196020772047,0.613390310441866,4.15371841694351));
#30346=CARTESIAN_POINT('Ctrl Pts',(9.08967604378332,0.202451179085494,4.59907474052783));
#30347=CARTESIAN_POINT('Ctrl Pts',(9.13739187984615,-0.394401985136886,
4.49429151193569));
#30348=CARTESIAN_POINT('Ctrl Pts',(9.18510771590899,-0.629069737753471,
3.93559278228048));
#30349=CARTESIAN_POINT('Ctrl Pts',(9.23282355197184,-0.28605307070895,3.43604019168954));
#30350=CARTESIAN_POINT('Ctrl Pts',(9.28053938803466,0.319650532659854,3.45438057070715));
#30351=CARTESIAN_POINT('Ctrl Pts',(9.32825522409751,0.631814133431458,3.97377166707843));
#30352=CARTESIAN_POINT('Ctrl Pts',(9.37597106016033,0.363773093762905,4.51724864514637));
#30353=CARTESIAN_POINT('Ctrl Pts',(9.4236868962232,-0.238326375276645,4.58572823348297));
#30354=CARTESIAN_POINT('Ctrl Pts',(9.47140273228601,-0.621567066777005,
4.11632457242483));
#30355=CARTESIAN_POINT('Ctrl Pts',(9.51911856834886,-0.434013156817378,
3.54009826662536));
#30356=CARTESIAN_POINT('Ctrl Pts',(9.5668344044117,0.152101713198456,3.38620679908157));
#30357=CARTESIAN_POINT('Ctrl Pts',(9.61455024047453,0.598539239598464,3.79597107236355));
#30358=CARTESIAN_POINT('Ctrl Pts',(9.66226607653739,0.495328972565208,4.39309824928265));
#30359=CARTESIAN_POINT('Ctrl Pts',(9.7099819126002,-0.0627495115905886,
4.62923725529147));
#30360=CARTESIAN_POINT('Ctrl Pts',(9.75769774866305,-0.563204153727404,
4.28753800770644));
#30361=CARTESIAN_POINT('Ctrl Pts',(9.80541358472588,-0.54645975548653,3.68178818330365));
#30362=CARTESIAN_POINT('Ctrl Pts',(9.85312942078873,-0.027892955418244,
3.36825716649128));
#30363=CARTESIAN_POINT('Ctrl Pts',(9.90084525685157,0.516288374798902,3.63486531430293));
#30364=CARTESIAN_POINT('Ctrl Pts',(9.9485610929144,0.58635414632045,4.2367822623095));
#30365=CARTESIAN_POINT('Ctrl Pts',(9.99627692897723,0.117961883057689,4.62125841547385));
#30366=CARTESIAN_POINT('Ctrl Pts',(10.0439927650401,-0.458756592493822,
4.4352234064191));
#30367=CARTESIAN_POINT('Ctrl Pts',(10.0917086011029,-0.614191830280748,
3.8495160464768));
#30368=CARTESIAN_POINT('Ctrl Pts',(10.1394244371658,-0.205605259764808,
3.40200041654811));
#30369=CARTESIAN_POINT('Ctrl Pts',(10.1871402732286,0.391791784436726,3.5036370055096));
#30370=CARTESIAN_POINT('Ctrl Pts',(10.2348561092915,0.629400404498524,4.06109136983801));
#30371=CARTESIAN_POINT('Ctrl Pts',(10.2825719453542,0.289020948539269,4.56244458923262));
#30372=CARTESIAN_POINT('Ctrl Pts',(10.3302877814171,-0.316770891622519,
4.54729628801251));
#30373=CARTESIAN_POINT('Ctrl Pts',(10.3780036174799,-0.631667147860668,
4.02955738427466));
#30374=CARTESIAN_POINT('Ctrl Pts',(10.4257194535428,-0.366493742769977,
3.48467547975859));
#30375=CARTESIAN_POINT('Ctrl Pts',(10.4734352896056,0.235236505537468,3.41302401146715));
#30376=CARTESIAN_POINT('Ctrl Pts',(10.5211511256685,0.620945451230968,3.88040162523195));
#30377=CARTESIAN_POINT('Ctrl Pts',(10.5688669617313,0.436430634585191,4.45760826680378));
#30378=CARTESIAN_POINT('Ctrl Pts',(10.6165827977941,-0.148865149148659,
4.61458619576145));
#30379=CARTESIAN_POINT('Ctrl Pts',(10.664298633857,-0.597455775834545,4.20718016452724));
#30380=CARTESIAN_POINT('Ctrl Pts',(10.7120144699198,-0.497393570532806,
3.60951740033105));
#30381=CARTESIAN_POINT('Ctrl Pts',(10.7597303059826,0.059432803973042,3.37044081575797));
#30382=CARTESIAN_POINT('Ctrl Pts',(10.8074461420455,0.56168112009921,3.70949811708754));
#30383=CARTESIAN_POINT('Ctrl Pts',(10.8551619781083,0.548129021063343,4.31532776744164));
#30384=CARTESIAN_POINT('Ctrl Pts',(10.9028778141712,0.0312216079359222,
4.63158707701274));
#30385=CARTESIAN_POINT('Ctrl Pts',(10.950593650234,-0.514357088165242,4.36785025554668));
#30386=CARTESIAN_POINT('Ctrl Pts',(10.9983094862968,-0.587593755803164,
3.7663108843084));
#30387=CARTESIAN_POINT('Ctrl Pts',(11.0460253223597,-0.12123403619496,3.37937182377895));
#30388=CARTESIAN_POINT('Ctrl Pts',(11.0937411584225,0.456456764276497,3.56236516706526));
#30389=CARTESIAN_POINT('Ctrl Pts',(11.1414569944854,0.61497629462275,4.14724531131301));
#30390=CARTESIAN_POINT('Ctrl Pts',(11.1891728305482,0.208753630990335,4.59690782052167));
#30391=CARTESIAN_POINT('Ctrl Pts',(11.236888666611,-0.389170704067994,4.49842069353791));
#30392=CARTESIAN_POINT('Ctrl Pts',(11.2846045026739,-0.629713593419695,
3.94222617449013));
#30393=CARTESIAN_POINT('Ctrl Pts',(11.3323203387367,-0.291980800545002,
3.43908624837263));
#30394=CARTESIAN_POINT('Ctrl Pts',(11.3800361747996,0.313882454172263,3.45104205114199));
#30395=CARTESIAN_POINT('Ctrl Pts',(11.4277520108624,0.631502621520784,3.96711438515144));
#30396=CARTESIAN_POINT('Ctrl Pts',(11.4754678469252,0.369204214609944,4.51338608528654));
#30397=CARTESIAN_POINT('Ctrl Pts',(11.5231836829881,-0.232140103514266,
4.58820744384271));
#30398=CARTESIAN_POINT('Ctrl Pts',(11.5708995190509,-0.620306592646703,
4.12286885598323));
#30399=CARTESIAN_POINT('Ctrl Pts',(11.6186153551137,-0.438835993107895,
3.54469790709399));
#30400=CARTESIAN_POINT('Ctrl Pts',(11.6663311911766,0.145624451261577,3.38463787584353));
#30401=CARTESIAN_POINT('Ctrl Pts',(11.7140470272394,0.596355721317347,3.78967435176932));
#30402=CARTESIAN_POINT('Ctrl Pts',(11.7617628633022,0.499444356375145,4.38785610674141));
#30403=CARTESIAN_POINT('Ctrl Pts',(11.8094786993651,-0.0561144459655822,
4.62986363095956));
#30404=CARTESIAN_POINT('Ctrl Pts',(11.8571945354279,-0.560142489144378,
4.29345769116983));
#30405=CARTESIAN_POINT('Ctrl Pts',(11.9049103714908,-0.549783065641843,
3.68756503815187));
#30406=CARTESIAN_POINT('Ctrl Pts',(11.9526262075536,-0.0345493934605723,
3.36858621802886));
#30407=CARTESIAN_POINT('Ctrl Pts',(12.0003420436164,0.512411518346294,3.62944438943981));
#30408=CARTESIAN_POINT('Ctrl Pts',(12.0480578796793,0.588817048391095,4.23058947975914));
#30409=CARTESIAN_POINT('Ctrl Pts',(12.0957737157421,0.1245028227835,4.61998070274044));
#30410=CARTESIAN_POINT('Ctrl Pts',(12.1434895518049,-0.454144260708352,
4.44003410676589));
#30411=CARTESIAN_POINT('Ctrl Pts',(12.1912053878678,-0.615743681684068,
3.85599741975318));
#30412=CARTESIAN_POINT('Ctrl Pts',(12.2389212239306,-0.211896205334937,
3.40420051794564));
#30413=CARTESIAN_POINT('Ctrl Pts',(12.2866370599935,0.386538816815474,3.49953544806202));
#30414=CARTESIAN_POINT('Ctrl Pts',(12.3343528960563,0.63000929582004,4.05445467686));
#30415=CARTESIAN_POINT('Ctrl Pts',(12.3820687321191,0.294932544534008,4.55936733800455));
#30416=CARTESIAN_POINT('Ctrl Pts',(12.429784568182,-0.310985300518122,4.55060436568669));
#30417=CARTESIAN_POINT('Ctrl Pts',(12.4775004042448,-0.631320558980542,
4.0362129322216));
#30418=CARTESIAN_POINT('Ctrl Pts',(12.5252162403077,-0.371904434015698,
3.48856660588983));
#30419=CARTESIAN_POINT('Ctrl Pts',(12.5729320763705,0.229037255191033,3.41057743478371));
#30420=CARTESIAN_POINT('Ctrl Pts',(12.6206479124333,0.619650508764677,3.87386407474765));
#30421=CARTESIAN_POINT('Ctrl Pts',(12.6683637484962,0.44122916559109,4.4529832757215));
#30422=CARTESIAN_POINT('Ctrl Pts',(12.716079584559,-0.142379709528176,4.61612096455669));
#30423=CARTESIAN_POINT('Ctrl Pts',(12.7637954206218,-0.595239106594286,
4.21346529139986));
#30424=CARTESIAN_POINT('Ctrl Pts',(12.8115112566847,-0.501481273143938,
3.61478115656484));
#30425=CARTESIAN_POINT('Ctrl Pts',(12.8592270927475,0.0527945297157079,
3.36984941301012));
#30426=CARTESIAN_POINT('Ctrl Pts',(12.9069429288104,0.558588303589165,3.70359464960132));
#30427=CARTESIAN_POINT('Ctrl Pts',(12.9546587648732,0.551421843290858,4.30953348024615));
#30428=CARTESIAN_POINT('Ctrl Pts',(13.002374600936,0.0378762195828894,4.63122295319618));
#30429=CARTESIAN_POINT('Ctrl Pts',(13.0500904369989,-0.510451719368595,
4.37325067561256));
#30430=CARTESIAN_POINT('Ctrl Pts',(13.0978062730617,-0.590023990114621,
3.77251655941407));
#30431=CARTESIAN_POINT('Ctrl Pts',(13.1455221091246,-0.127768152052348,
3.38068398698829));
#30432=CARTESIAN_POINT('Ctrl Pts',(13.1932379451874,0.451819146005312,3.55757883871291));
#30433=CARTESIAN_POINT('Ctrl Pts',(13.2409537812502,0.616493970155128,4.14075585037205));
#30434=CARTESIAN_POINT('Ctrl Pts',(13.2886696173131,0.215032895532453,4.59467459882739));
#30435=CARTESIAN_POINT('Ctrl Pts',(13.3363854533759,-0.383896195764066,
4.50249451293469));
#30436=CARTESIAN_POINT('Ctrl Pts',(13.3841012894387,-0.630287503488198,
3.94886598394213));
#30437=CARTESIAN_POINT('Ctrl Pts',(13.4318171255016,-0.297876098539286,
3.4421946086935));
#30438=CARTESIAN_POINT('Ctrl Pts',(13.4795329615644,0.308079511111167,3.44776450722078));
#30439=CARTESIAN_POINT('Ctrl Pts',(13.5272487976272,0.631120965295637,3.96046075600252));
#30440=CARTESIAN_POINT('Ctrl Pts',(13.5749646336901,0.374594326004835,4.50946650093658));
#30441=CARTESIAN_POINT('Ctrl Pts',(13.6226804697529,-0.225928046730791,
4.59062131891086));
#30442=CARTESIAN_POINT('Ctrl Pts',(13.6703963058158,-0.618977217803688,
4.12939949185215));
#30443=CARTESIAN_POINT('Ctrl Pts',(13.7181121418786,-0.443610085578744,
3.54934812035851));
#30444=CARTESIAN_POINT('Ctrl Pts',(13.7658279779415,0.139131014051702,3.38313730411011));
#30445=CARTESIAN_POINT('Ctrl Pts',(13.8135438140043,0.594105962672646,3.78340099315002));
#30446=CARTESIAN_POINT('Ctrl Pts',(13.8612596500671,0.503504264276035,4.38257088298437));
#30447=CARTESIAN_POINT('Ctrl Pts',(13.90897548613,-0.0494731474142026,4.63042004436449));
#30448=CARTESIAN_POINT('Ctrl Pts',(13.9566913221928,-0.557018606591754,
4.29934477874546));
#30449=CARTESIAN_POINT('Ctrl Pts',(14.0044071582556,-0.553045308503159,
3.69337659679301));
#30450=CARTESIAN_POINT('Ctrl Pts',(14.0521229943185,-0.0412019939202257,
3.36898540401303));
#30451=CARTESIAN_POINT('Ctrl Pts',(14.0998388303813,0.50847774565382,3.62406462413548));
#30452=CARTESIAN_POINT('Ctrl Pts',(14.1475546664442,0.591214547458171,4.22437108442359));
#30453=CARTESIAN_POINT('Ctrl Pts',(14.195270502507,0.131029933326566,4.61863412549262));
#30454=CARTESIAN_POINT('Ctrl Pts',(14.2429863385698,-0.4494814847335,4.44479593021223));
#30455=CARTESIAN_POINT('Ctrl Pts',(14.2907021746327,-0.617227139201166,
3.86249478815283));
#30456=CARTESIAN_POINT('Ctrl Pts',(14.3384180106955,-0.218163614480107,
3.40646679792233));
#30457=CARTESIAN_POINT('Ctrl Pts',(14.3861338467583,0.381242914296727,3.49548947984197));
#30458=CARTESIAN_POINT('Ctrl Pts',(14.4338496828212,0.630548208698617,4.0478119353149));
#30459=CARTESIAN_POINT('Ctrl Pts',(14.481565518884,0.300811380821271,4.55622795490698));
#30460=CARTESIAN_POINT('Ctrl Pts',(14.5292813549469,-0.305165166642291,
4.55385128484077));
#30461=CARTESIAN_POINT('Ctrl Pts',(14.5769971910097,-0.630903846008588,
4.04286445780787));
#30462=CARTESIAN_POINT('Ctrl Pts',(14.6247130270726,-0.37727381588172,3.49251453961553));
#30463=CARTESIAN_POINT('Ctrl Pts',(14.6724288631354,0.222812564473163,3.40819632836178));
#30464=CARTESIAN_POINT('Ctrl Pts',(14.7201446991982,0.618286738460357,3.86734053484336));
#30465=CARTESIAN_POINT('Ctrl Pts',(14.7678605352611,0.44597868695508,4.44830796940654));
#30466=CARTESIAN_POINT('Ctrl Pts',(14.8155763713239,-0.135878455045208,
4.6175872975589));
#30467=CARTESIAN_POINT('Ctrl Pts',(14.8632922073867,-0.592956321018707,
4.2197267075609));
#30468=CARTESIAN_POINT('Ctrl Pts',(14.9110080434496,-0.505513273594975,
3.62008770107973));
#30469=CARTESIAN_POINT('Ctrl Pts',(14.9587238795124,0.0461503912925444,
3.36932800439917));
#30470=CARTESIAN_POINT('Ctrl Pts',(15.0064397155752,0.555433441741075,3.69772410541485));
#30471=CARTESIAN_POINT('Ctrl Pts',(15.0541555516381,0.554653416196733,4.30370481154056));
#30472=CARTESIAN_POINT('Ctrl Pts',(15.1018713877009,0.0445266241191229,
4.63078871612938));
#30473=CARTESIAN_POINT('Ctrl Pts',(15.1495872237638,-0.506489652017253,
4.37860963676461));
#30474=CARTESIAN_POINT('Ctrl Pts',(15.1973030598266,-0.592388687361149,
3.77874750230084));
#30475=CARTESIAN_POINT('Ctrl Pts',(15.2450188958894,-0.134288076029725,
3.38206494088146));
#30476=CARTESIAN_POINT('Ctrl Pts',(15.2927347319523,0.447131341807447,3.5528416524037));
#30477=CARTESIAN_POINT('Ctrl Pts',(15.3404505680151,0.617943168462805,4.13425075493917));
#30478=CARTESIAN_POINT('Ctrl Pts',(15.3881664040779,0.221288275240951,4.59237532350063));
#30479=CARTESIAN_POINT('Ctrl Pts',(15.4358822401408,-0.378579046092452,
4.50651251762549));
#30480=CARTESIAN_POINT('Ctrl Pts',(15.4835980762036,-0.630791404211772,
3.95551147311801));
#30481=CARTESIAN_POINT('Ctrl Pts',(15.5313139122665,-0.303738309870084,
3.44536492739022));
#30482=CARTESIAN_POINT('Ctrl Pts',(15.5790297483293,0.302242348039936,3.44454830299756));
#30483=CARTESIAN_POINT('Ctrl Pts',(15.6267455843921,0.630669207148581,3.95381151868517));
#30484=CARTESIAN_POINT('Ctrl Pts',(15.674461420455,0.379942829239589,4.50549032746533));
#30485=CARTESIAN_POINT('Ctrl Pts',(15.7221772565178,-0.219690894932002,
4.59296959056563));
#30486=CARTESIAN_POINT('Ctrl Pts',(15.7698930925806,-0.617579089908608,
4.13591575463957));
#30487=CARTESIAN_POINT('Ctrl Pts',(15.8176089286435,-0.448334903946386,
3.5540483898953));
#30488=CARTESIAN_POINT('Ctrl Pts',(15.8653247647063,0.13262212282903,3.3817052505577));
#30489=CARTESIAN_POINT('Ctrl Pts',(15.9130406007692,0.591790213556878,3.77715169332057));
#30490=CARTESIAN_POINT('Ctrl Pts',(15.960756436832,0.507508245312566,4.37724316506909));
#30491=CARTESIAN_POINT('Ctrl Pts',(16.0084722728949,-0.0428263536203826,
4.63090643370248));
#30492=CARTESIAN_POINT('Ctrl Pts',(16.0561881089577,-0.553832853055588,
4.30519861652357));
#30493=CARTESIAN_POINT('Ctrl Pts',(16.1039039450205,-0.556246121716014,
3.69922221370673));
#30494=CARTESIAN_POINT('Ctrl Pts',(16.1516197810833,-0.0478500178579074,
3.36945468010413));
#30495=CARTESIAN_POINT('Ctrl Pts',(16.1993356171462,0.504487493666278,3.61872661594874));
#30496=CARTESIAN_POINT('Ctrl Pts',(16.247051453209,0.593546377218863,4.21812776701271));
#30497=CARTESIAN_POINT('Ctrl Pts',(16.2947672892719,0.137542489686435,4.61721883330181));
#30498=CARTESIAN_POINT('Ctrl Pts',(16.3424831253347,-0.444768782488292,
4.44950834783736));
#30499=CARTESIAN_POINT('Ctrl Pts',(16.3901989613976,-0.618642038056621,
3.86900742997889));
#30500=CARTESIAN_POINT('Ctrl Pts',(16.4379147974604,-0.224406791046256,
3.40879900475058));
#30501=CARTESIAN_POINT('Ctrl Pts',(16.4856306335233,0.375904665124208,3.49149955025639));
#30502=CARTESIAN_POINT('Ctrl Pts',(16.533346469586,0.631017083274371,4.04116388304691));
#30503=CARTESIAN_POINT('Ctrl Pts',(16.5810623056489,0.306656804407812,4.55302678864769));
#30504=CARTESIAN_POINT('Ctrl Pts',(16.6287781417117,-0.29931113646787,4.55703668482238));
#30505=CARTESIAN_POINT('Ctrl Pts',(16.6764939777746,-0.630417055231307,
4.04951122221356));
#30506=CARTESIAN_POINT('Ctrl Pts',(16.7242098138374,-0.382601291962586,
3.49651884241796));
#30507=CARTESIAN_POINT('Ctrl Pts',(16.7719256499003,0.216563124792967,3.40588095668335));
#30508=CARTESIAN_POINT('Ctrl Pts',(16.8196414859631,0.616854291799135,3.86083173012294));
#30509=CARTESIAN_POINT('Ctrl Pts',(16.8673573220259,0.450678671122871,4.44358286716973));
#30510=CARTESIAN_POINT('Ctrl Pts',(16.9150731580887,-0.129362107828251,
4.61898503189482));
#30511=CARTESIAN_POINT('Ctrl Pts',(16.9627889941516,-0.590607672668797,
4.22596371752193));
#30512=CARTESIAN_POINT('Ctrl Pts',(17.0105048302144,-0.509489124030439,
3.62543644444997));
#30513=CARTESIAN_POINT('Ctrl Pts',(17.0582206662773,0.0395011267029154,
3.3688766478407));
#30514=CARTESIAN_POINT('Ctrl Pts',(17.1059365023401,0.552216884982031,3.69188713660034));
#30515=CARTESIAN_POINT('Ctrl Pts',(17.153652338403,0.557823380833178,4.29784240874569));
#30516=CARTESIAN_POINT('Ctrl Pts',(17.2013681744658,0.0511720828492506,
4.63028441404532));
#30517=CARTESIAN_POINT('Ctrl Pts',(17.2490840105287,-0.502471326198846,
4.38392654375487));
#30518=CARTESIAN_POINT('Ctrl Pts',(17.2967998465914,-0.594687584883411,
3.78500302086511));
#30519=CARTESIAN_POINT('Ctrl Pts',(17.3445156826543,-0.140793083924855,
3.38351453206865));
#30520=CARTESIAN_POINT('Ctrl Pts',(17.3922315187171,0.442393872381948,3.5481541343218));
#30521=CARTESIAN_POINT('Ctrl Pts',(17.43994735478,0.61932372857571,4.1277307475695));
#30522=CARTESIAN_POINT('Ctrl Pts',(17.4876631908428,0.227519075297936,4.590010249934));
#30523=CARTESIAN_POINT('Ctrl Pts',(17.5353790269057,-0.373219845656906,
4.51047426130944));
#30524=CARTESIAN_POINT('Ctrl Pts',(17.5830948629685,-0.631225239619516,
3.96216190386831));
#30525=CARTESIAN_POINT('Ctrl Pts',(17.6308106990313,-0.309566783390781,
3.44859685231885));
#30526=CARTESIAN_POINT('Ctrl Pts',(17.6785265350942,0.29637161332294,3.44139379571298));
#30527=CARTESIAN_POINT('Ctrl Pts',(17.726242371157,0.630147397258769,3.94716741176515));
#30528=CARTESIAN_POINT('Ctrl Pts',(17.7739582072198,0.385249130227842,4.50145800652724));
#30529=CARTESIAN_POINT('Ctrl Pts',(17.8216740432827,-0.213429340911116,
4.59525199797214));
#30530=CARTESIAN_POINT('Ctrl Pts',(17.8693898793456,-0.616112364258878,
4.14241692054995));
#30531=CARTESIAN_POINT('Ctrl Pts',(17.9171057154084,-0.453009923400427,
3.55879819362073));
#30532=CARTESIAN_POINT('Ctrl Pts',(17.9648215514712,0.126098500570276,3.38034187425201));
#30533=CARTESIAN_POINT('Ctrl Pts',(18.012537387534,0.589408731192455,3.77092714642348));
#30534=CARTESIAN_POINT('Ctrl Pts',(18.0602532235969,0.511455854741549,4.3718735447732));
#30535=CARTESIAN_POINT('Ctrl Pts',(18.1079690596597,-0.0361748028784226,
4.6313227449477));
#30536=CARTESIAN_POINT('Ctrl Pts',(18.1556848957226,-0.55058558239424,4.31101855428765));
#30537=CARTESIAN_POINT('Ctrl Pts',(18.2034007317854,-0.559385149749292,
3.70510123958967));
#30538=CARTESIAN_POINT('Ctrl Pts',(18.2511165678482,-0.0544927268426965,
3.36999399417717));
#30539=CARTESIAN_POINT('Ctrl Pts',(18.2988324039111,0.500441205601937,3.6134309578002));
#30540=CARTESIAN_POINT('Ctrl Pts',(18.3465482399739,0.595812278664582,4.21186022100458));
#30541=CARTESIAN_POINT('Ctrl Pts',(18.3942640760367,0.144039768479226,4.61573498337195));
#30542=CARTESIAN_POINT('Ctrl Pts',(18.4419799120996,-0.440006677437314,
4.4541708362083));
#30543=CARTESIAN_POINT('Ctrl Pts',(18.4896957481624,-0.619988221090196,
3.87553462183804));
#30544=CARTESIAN_POINT('Ctrl Pts',(18.5374115842252,-0.230625041570952,
3.41119687937986));
#30545=CARTESIAN_POINT('Ctrl Pts',(18.5851274202881,0.370524662245315,3.48756610248778));
#30546=CARTESIAN_POINT('Ctrl Pts',(18.6328432563509,0.631415867466904,4.03451125849008));
#30547=CARTESIAN_POINT('Ctrl Pts',(18.6805590924138,0.31246816601179,4.54976419479712));
#30548=CARTESIAN_POINT('Ctrl Pts',(18.7282749284766,-0.293423860232864,
4.56016021181225));
#30549=CARTESIAN_POINT('Ctrl Pts',(18.7759907645394,-0.629860240718928,
4.05615248714788));
#30550=CARTESIAN_POINT('Ctrl Pts',(18.8237066006023,-0.387886270507855,
3.50057906951772));
#30551=CARTESIAN_POINT('Ctrl Pts',(18.8714224366651,0.210289630309142,3.40363157692976));
#30552=CARTESIAN_POINT('Ctrl Pts',(18.919138272728,0.615353327889266,3.85433838355196));
#30553=CARTESIAN_POINT('Ctrl Pts',(18.9668541087908,0.455328596044662,4.43880849385601));
#30554=CARTESIAN_POINT('Ctrl Pts',(19.0145699448537,-0.122831391686292,
4.62031401230505));
#30555=CARTESIAN_POINT('Ctrl Pts',(19.0622857809165,-0.588193422413584,
4.2321756285162));
#30556=CARTESIAN_POINT('Ctrl Pts',(19.1100016169793,-0.513408382846255,
3.63082679254236));
#30557=CARTESIAN_POINT('Ctrl Pts',(19.1577174530421,0.0328474745430158,
3.36849539350727));
#30558=CARTESIAN_POINT('Ctrl Pts',(19.205433289105,0.548938990540088,3.68608439142882));
#30559=CARTESIAN_POINT('Ctrl Pts',(19.2531491251678,0.560931385193363,4.2919469231649));
#30560=CARTESIAN_POINT('Ctrl Pts',(19.3008649612307,0.0578118574426247,
4.62971010270368));
#30561=CARTESIAN_POINT('Ctrl Pts',(19.3485807972935,-0.498397187901359,
4.38920080648958));
#30562=CARTESIAN_POINT('Ctrl Pts',(19.3962966333563,-0.596920427988996,
3.79128241936144));
#30563=CARTESIAN_POINT('Ctrl Pts',(19.4440124694192,-0.147282451949449,
3.38503260125846));
#30564=CARTESIAN_POINT('Ctrl Pts',(19.491728305482,0.437607261597584,3.54351680188243));
#30565=CARTESIAN_POINT('Ctrl Pts',(19.5394441415449,0.620635501579114,4.12119655861503));
#30566=CARTESIAN_POINT('Ctrl Pts',(19.5871599776077,0.233724595248439,4.58757962923414));
#30567=CARTESIAN_POINT('Ctrl Pts',(19.6348758136705,-0.367819173932889,
4.51437932582758));
#30568=CARTESIAN_POINT('Ctrl Pts',(19.6825916497334,-0.631588991354928,
3.96881649615688));
#30569=CARTESIAN_POINT('Ctrl Pts',(19.7303074857962,-0.315360815373557,
3.4518901025469));
#30570=CARTESIAN_POINT('Ctrl Pts',(19.778023321859,0.290467852693633,3.43830118837221));
#30571=CARTESIAN_POINT('Ctrl Pts',(19.8257391579219,0.629555794415491,3.94052945152661));
#30572=CARTESIAN_POINT('Ctrl Pts',(19.8734549939847,0.390512260364629,4.49736946054851));
#30573=CARTESIAN_POINT('Ctrl Pts',(19.9211708300476,-0.207143364153331,
4.59746927979605));
#30574=CARTESIAN_POINT('Ctrl Pts',(19.9688866661104,-0.61457855576007,4.14890039401813));
#30575=CARTESIAN_POINT('Ctrl Pts',(20.0166025021732,-0.45763207183192,3.5636005413983));
#30576=CARTESIAN_POINT('Ctrl Pts',(20.0643183382361,0.119556051622903,3.37904064719698));
#30577=CARTESIAN_POINT('Ctrl Pts',(20.1120341742989,0.586970881772813,3.7647406560623));
#30578=CARTESIAN_POINT('Ctrl Pts',(20.1597500103618,0.515329468049299,4.36643880344312));
#30579=CARTESIAN_POINT('Ctrl Pts',(20.2074658464246,-0.029486781418557,
4.63171390504007));
#30580=CARTESIAN_POINT('Ctrl Pts',(20.2551816824874,-0.547338447674763,
4.31671898245684));
#30581=CARTESIAN_POINT('Ctrl Pts',(20.3028975185503,-0.562346186529673,
3.71117381387971));
#30582=CARTESIAN_POINT('Ctrl Pts',(20.3506133546131,-0.0613491664957494,
3.37029669484294));
#30583=CARTESIAN_POINT('Ctrl Pts',(20.398329190676,0.496762641213801,3.60878154740643));
#30584=CARTESIAN_POINT('Ctrl Pts',(20.4380923873949,0.580417208789547,4.10498761157686));
#30585=CARTESIAN_POINT('Ctrl Pts',(20.4699029447702,0.374745574175769,4.41137453781958));
#30586=CARTESIAN_POINT('Ctrl Pts',(20.4937608628016,0.13332385162888,4.54159545884303));
#30587=CARTESIAN_POINT('Ctrl Pts',(20.517618780833,-0.143293564288956,4.53872805560682));
#30588=CARTESIAN_POINT('Ctrl Pts',(20.5414766988645,-0.38346854803195,4.40448715909776));
#30589=CARTESIAN_POINT('Ctrl Pts',(20.5653346168959,-0.530621786340447,
4.17114564603877));
#30590=CARTESIAN_POINT('Ctrl Pts',(20.5891925349273,-0.547627617499454,
3.89605651468078));
#30591=CARTESIAN_POINT('Ctrl Pts',(20.6130504529587,-0.430933317123153,
3.64633026976583));
#30592=CARTESIAN_POINT('Ctrl Pts',(20.6369083709901,-0.208752997660079,
3.48311457674551));
#30593=CARTESIAN_POINT('Ctrl Pts',(20.6607662890215,0.0644142843662171,
3.4462762657402));
#30594=CARTESIAN_POINT('Ctrl Pts',(20.684624207053,0.321861676845817,3.54484653226013));
#30595=CARTESIAN_POINT('Ctrl Pts',(20.7084821250844,0.500588620804837,3.75470996102831));
#30596=CARTESIAN_POINT('Ctrl Pts',(20.7323400431158,0.556916750317041,4.02455574134091));
#30597=CARTESIAN_POINT('Ctrl Pts',(20.7561979611472,0.47705893600668,4.28839577951569));
#30598=CARTESIAN_POINT('Ctrl Pts',(20.7800558791787,0.280549668164313,4.48171582646486));
#30599=CARTESIAN_POINT('Ctrl Pts',(20.8039137972101,0.0154370662995263,
4.55724289713534));
#30600=CARTESIAN_POINT('Ctrl Pts',(20.8277717152415,-0.253449631274377,
4.49650907789895));
#30601=CARTESIAN_POINT('Ctrl Pts',(20.8516296332729,-0.460361354274216,
4.31436517051053));
#30602=CARTESIAN_POINT('Ctrl Pts',(20.8754875513043,-0.554701993332711,
4.05535046556385));
#30603=CARTESIAN_POINT('Ctrl Pts',(20.8993454693358,-0.513402987365846,
3.78280103771366));
#30604=CARTESIAN_POINT('Ctrl Pts',(20.9232033873672,-0.346562912086465,
3.56336268648205));
#30605=CARTESIAN_POINT('Ctrl Pts',(20.9470613053986,-0.0949787932613798,
3.45069404477467));
#30606=CARTESIAN_POINT('Ctrl Pts',(20.97091922343,0.179830242856268,3.47234567582879));
#30607=CARTESIAN_POINT('Ctrl Pts',(20.9947771414614,0.410665878084123,3.62302316008453));
#30608=CARTESIAN_POINT('Ctrl Pts',(21.0186350594928,0.541082524061315,3.86588175144064));
#30609=CARTESIAN_POINT('Ctrl Pts',(21.0424929775243,0.539189751860116,4.14153590729571));
#30610=CARTESIAN_POINT('Ctrl Pts',(21.0663508955557,0.405450399288564,4.38258067876424));
#30611=CARTESIAN_POINT('Ctrl Pts',(21.0902088135871,0.172567379211795,4.53007405282339));
#30612=CARTESIAN_POINT('Ctrl Pts',(21.1140667316185,-0.102513065388571,
4.54794988212627));
#30613=CARTESIAN_POINT('Ctrl Pts',(21.1379246496499,-0.352526273278862,
4.43183703934844));
#30614=CARTESIAN_POINT('Ctrl Pts',(21.1617825676814,-0.516337204635697,
4.21012827746935));
#30615=CARTESIAN_POINT('Ctrl Pts',(21.1856404857128,-0.553889624765765,
3.93703742795684));
#30616=CARTESIAN_POINT('Ctrl Pts',(21.2094984037442,-0.456000943963824,
3.67934264238169));
#30617=CARTESIAN_POINT('Ctrl Pts',(21.2333563217756,-0.246607611160355,
3.50005731527167));
#30618=CARTESIAN_POINT('Ctrl Pts',(21.257214239807,0.0230880000356606,3.44302159274494));
#30619=CARTESIAN_POINT('Ctrl Pts',(21.2810721578385,0.287137966314551,3.52218226257825));
#30620=CARTESIAN_POINT('Ctrl Pts',(21.3049300758698,0.480974878350452,3.71818238470557));
#30621=CARTESIAN_POINT('Ctrl Pts',(21.3287879939013,0.557200331135927,3.9830945903298));
#30622=CARTESIAN_POINT('Ctrl Pts',(21.3526459119327,0.497175125126959,4.25214062911267));
#30623=CARTESIAN_POINT('Ctrl Pts',(21.3765038299641,0.31557705824565,4.45953141590455));
#30624=CARTESIAN_POINT('Ctrl Pts',(21.4003617479955,0.0568118044769688,
4.55455425412338));
#30625=CARTESIAN_POINT('Ctrl Pts',(21.424219666027,-0.215845483008899,4.51397347145443));
#30626=CARTESIAN_POINT('Ctrl Pts',(21.4480775840584,-0.435722670386138,
4.34771217465862));
#30627=CARTESIAN_POINT('Ctrl Pts',(21.4719355020898,-0.549053796006754,
4.0964257796693));
#30628=CARTESIAN_POINT('Ctrl Pts',(21.4957934201212,-0.528126312578589,
3.82156065496534));
#30629=CARTESIAN_POINT('Ctrl Pts',(21.5196513381527,-0.378057559853047,
3.59032881071252));
#30630=CARTESIAN_POINT('Ctrl Pts',(21.543509256184,-0.135543435662257,3.45927273145963));
#30631=CARTESIAN_POINT('Ctrl Pts',(21.5673671742155,0.14011475067701,3.46043919847993));
#30632=CARTESIAN_POINT('Ctrl Pts',(21.5912250922469,0.381511063826562,3.59354297881304));
#30633=CARTESIAN_POINT('Ctrl Pts',(21.6150830102783,0.529617529717794,3.8260365724933));
#30634=CARTESIAN_POINT('Ctrl Pts',(21.6389409283097,0.548218083101175,4.10106896286759));
#30635=CARTESIAN_POINT('Ctrl Pts',(21.6627988463412,0.432764382005563,4.35138723875747));
#30636=CARTESIAN_POINT('Ctrl Pts',(21.6866567643726,0.211488001244504,4.51578176317496));
#30637=CARTESIAN_POINT('Ctrl Pts',(21.710514682404,-0.0615029566383307,
4.55405359688301));
#30638=CARTESIAN_POINT('Ctrl Pts',(21.7343726004354,-0.319454766316188,
4.4568442340362));
#30639=CARTESIAN_POINT('Ctrl Pts',(21.7582305184669,-0.499291183856609,
4.24792401178047));
#30640=CARTESIAN_POINT('Ctrl Pts',(21.7820884364982,-0.557037306525311,
3.97837961532992));
#30641=CARTESIAN_POINT('Ctrl Pts',(21.8059463545297,-0.478572634356998,
3.71412199185867));
#30642=CARTESIAN_POINT('Ctrl Pts',(21.8298042725611,-0.283083917031579,
3.51976932853855));
#30643=CARTESIAN_POINT('Ctrl Pts',(21.8536621905926,-0.018373470940863,
3.44284614561161));
#30644=CARTESIAN_POINT('Ctrl Pts',(21.8775201086239,0.250829789278194,3.5021622566489));
#30645=CARTESIAN_POINT('Ctrl Pts',(21.9013780266554,0.458698333552465,3.68321325676341));
#30646=CARTESIAN_POINT('Ctrl Pts',(21.9252359446868,0.55440264058141,3.94172724469688));
#30647=CARTESIAN_POINT('Ctrl Pts',(21.9490938627182,0.514540400363477,4.21449050861997));
#30648=CARTESIAN_POINT('Ctrl Pts',(21.9729517807496,0.348859016457567,4.4348050005813));
#30649=CARTESIAN_POINT('Ctrl Pts',(21.996809698781,0.0978721002989983,4.54879782605011));
#30650=CARTESIAN_POINT('Ctrl Pts',(22.0206676168125,-0.177047210365213,
4.52859463409701));
#30651=CARTESIAN_POINT('Ctrl Pts',(22.0445255348439,-0.408673655425848,
4.3791356554785));
#30652=CARTESIAN_POINT('Ctrl Pts',(22.0683834528753,-0.540368259688198,
4.13696768164748));
#30653=CARTESIAN_POINT('Ctrl Pts',(22.0922413709067,-0.53992810512055,3.86130737872913));
#30654=CARTESIAN_POINT('Ctrl Pts',(22.1160992889381,-0.407460821505317,
3.61956119962225));
#30655=CARTESIAN_POINT('Ctrl Pts',(22.1399572069695,-0.175358268020808,
3.47084267015335));
#30656=CARTESIAN_POINT('Ctrl Pts',(22.163815125001,0.0996241586556461,3.45151752178681));
#30657=CARTESIAN_POINT('Ctrl Pts',(22.1876730430324,0.350245764837839,3.56631127970877));
#30658=CARTESIAN_POINT('Ctrl Pts',(22.2115309610638,0.51522274100534,3.78715374318048));
#30659=CARTESIAN_POINT('Ctrl Pts',(22.2353888790952,0.554213722627899,4.06004291426965));
#30660=CARTESIAN_POINT('Ctrl Pts',(22.2592467971266,0.457684352558003,4.31824995726588));
#30661=CARTESIAN_POINT('Ctrl Pts',(22.2831047151581,0.249238691275201,4.49863621678958));
#30662=CARTESIAN_POINT('Ctrl Pts',(22.3069626331895,-0.0201526192614011,
4.55709233866662));
#30663=CARTESIAN_POINT('Ctrl Pts',(22.3308205512209,-0.284616065231974,
4.47932420896945));
#30664=CARTESIAN_POINT('Ctrl Pts',(22.3546784692523,-0.479483130864429,
4.28434825342259));
#30665=CARTESIAN_POINT('Ctrl Pts',(22.3785363872838,-0.557103509392546,
4.01984140485232));
#30666=CARTESIAN_POINT('Ctrl Pts',(22.4023943053151,-0.498496906094933,
3.75048279151596));
#30667=CARTESIAN_POINT('Ctrl Pts',(22.4262522233466,-0.317994227800984,
3.542137933897));
#30668=CARTESIAN_POINT('Ctrl Pts',(22.450110141378,-0.0597333038680864,
3.44575282046209));
#30669=CARTESIAN_POINT('Ctrl Pts',(22.4739680594094,0.213134049493302,3.48489624527193));
#30670=CARTESIAN_POINT('Ctrl Pts',(22.4978259774408,0.433884304103661,3.6499965589521));
#30671=CARTESIAN_POINT('Ctrl Pts',(22.5216838954723,0.548538061567711,3.90068226732924));
#30672=CARTESIAN_POINT('Ctrl Pts',(22.5455418135037,0.529059256943919,4.17565382996358));
#30673=CARTESIAN_POINT('Ctrl Pts',(22.5693997315351,0.380211173855379,4.40767331583304));
#30674=CARTESIAN_POINT('Ctrl Pts',(22.5932576495665,0.138390873272415,4.54000544018811));
#30675=CARTESIAN_POINT('Ctrl Pts',(22.6171155675979,-0.137269333605106,
4.54029177230974));
#30676=CARTESIAN_POINT('Ctrl Pts',(22.6409734856293,-0.379364264814148,
4.40846158181013));
#30677=CARTESIAN_POINT('Ctrl Pts',(22.6648314036608,-0.528692759685234,
4.17675229015827));
#30678=CARTESIAN_POINT('Ctrl Pts',(22.6886893216921,-0.54874438127821,3.90182058373076));
#30679=CARTESIAN_POINT('Ctrl Pts',(22.7125472397236,-0.434607562942265,
3.65089956353622));
#30680=CARTESIAN_POINT('Ctrl Pts',(22.736405157755,-0.214207731687487,3.48533716867003));
#30681=CARTESIAN_POINT('Ctrl Pts',(22.7602630757864,0.0585913648593265,
3.44563509732658));
#30682=CARTESIAN_POINT('Ctrl Pts',(22.7841209938179,0.31702578011682,3.5414689143437));
#30683=CARTESIAN_POINT('Ctrl Pts',(22.8079789118493,0.498012898707086,3.74946820019106));
#30684=CARTESIAN_POINT('Ctrl Pts',(22.8238841905369,0.537376264140017,3.92891364167179));
#30685=CARTESIAN_POINT('Ctrl Pts',(22.8318368298807,0.534391234777113,4.01792167950194));
#30686=CARTESIAN_POINT('Ctrl Pts',(3.99999999999998,0.254694598474614,4.53673594206822));
#30687=CARTESIAN_POINT('Ctrl Pts',(4.00795263934379,0.165296026927429,4.57915779516171));
#30688=CARTESIAN_POINT('Ctrl Pts',(4.0238579180314,-0.0350146299391769,
4.61842892627033));
#30689=CARTESIAN_POINT('Ctrl Pts',(4.04771583606282,-0.327086058023631,
4.5259865276721));
#30690=CARTESIAN_POINT('Ctrl Pts',(4.07157375409423,-0.539100294705402,
4.30498302442502));
#30691=CARTESIAN_POINT('Ctrl Pts',(4.09543167212566,-0.619328256935644,
4.00937412827253));
#30692=CARTESIAN_POINT('Ctrl Pts',(4.11928959015708,-0.548093442686671,
3.71148804617917));
#30693=CARTESIAN_POINT('Ctrl Pts',(4.1431475081885,-0.342845496867427,3.48414304986991));
#30694=CARTESIAN_POINT('Ctrl Pts',(4.16700542621991,-0.0537568536316998,
3.38294333505492));
#30695=CARTESIAN_POINT('Ctrl Pts',(4.19086334425134,0.248473820944083,3.43262855616194));
#30696=CARTESIAN_POINT('Ctrl Pts',(4.21472126228276,0.489947458130694,3.62105272953394));
#30697=CARTESIAN_POINT('Ctrl Pts',(4.23857918031417,0.611614759069978,3.90213920826301));
#30698=CARTESIAN_POINT('Ctrl Pts',(4.26243709834559,0.583726034554802,4.20715564703007));
#30699=CARTESIAN_POINT('Ctrl Pts',(4.28629501637702,0.413100159498109,4.46151671210738));
#30700=CARTESIAN_POINT('Ctrl Pts',(4.31015293440843,0.141460167127662,4.60302446238992));
#30701=CARTESIAN_POINT('Ctrl Pts',(4.33401085243986,-0.164770755236008,
4.59707625642582));
#30702=CARTESIAN_POINT('Ctrl Pts',(4.35786877047126,-0.430710704813839,
4.44512666775742));
#30703=CARTESIAN_POINT('Ctrl Pts',(4.38172668850269,-0.59133017320549,4.18433147003372));
#30704=CARTESIAN_POINT('Ctrl Pts',(4.40558460653411,-0.607353296958831,
3.87846221409715));
#30705=CARTESIAN_POINT('Ctrl Pts',(4.42944252456553,-0.474862000813124,
3.60231225357117));
#30706=CARTESIAN_POINT('Ctrl Pts',(4.45330044259694,-0.226254007744579,
3.42340778189093));
#30707=CARTESIAN_POINT('Ctrl Pts',(4.47715836062837,0.0776792518003291,
3.38549581251083));
#30708=CARTESIAN_POINT('Ctrl Pts',(4.50101627865978,0.362617819109035,3.49784685630402));
#30709=CARTESIAN_POINT('Ctrl Pts',(4.5248741966912,0.558886451727075,3.73298802180378));
#30710=CARTESIAN_POINT('Ctrl Pts',(4.54873211472262,0.618492123352341,4.03342088939383));
#30711=CARTESIAN_POINT('Ctrl Pts',(4.57259003275404,0.5268596233165,4.32568143907503));
#30712=CARTESIAN_POINT('Ctrl Pts',(4.59644795078546,0.306395594072305,4.5383040055633));
#30713=CARTESIAN_POINT('Ctrl Pts',(4.62030586881688,0.0110094959969652,
4.61929657956068));
#30714=CARTESIAN_POINT('Ctrl Pts',(4.6441637868483,-0.287068723725306,4.54885427056805));
#30715=CARTESIAN_POINT('Ctrl Pts',(4.66802170487971,-0.514950820910697,
4.34420214192463));
#30716=CARTESIAN_POINT('Ctrl Pts',(4.69187962291114,-0.616913415399932,
4.05538321370614));
#30717=CARTESIAN_POINT('Ctrl Pts',(4.71573754094255,-0.568023875442366,
3.75302158112612));
#30718=CARTESIAN_POINT('Ctrl Pts',(4.73959545897398,-0.380237025278099,
3.51105289951885));
#30719=CARTESIAN_POINT('Ctrl Pts',(4.76345337700539,-0.0994718649854296,
3.38864510263028));
#30720=CARTESIAN_POINT('Ctrl Pts',(4.78731129503681,0.205616875855751,3.41573023112194));
#30721=CARTESIAN_POINT('Ctrl Pts',(4.81116921306823,0.460426689658758,3.5856852332931));
#30722=CARTESIAN_POINT('Ctrl Pts',(4.83502713109965,0.60264963606909,3.85695148163183));
#30723=CARTESIAN_POINT('Ctrl Pts',(4.85888504913107,0.597508330613982,4.16319698927494));
#30724=CARTESIAN_POINT('Ctrl Pts',(4.88274296716248,0.446259962523644,4.42953638764361));
#30725=CARTESIAN_POINT('Ctrl Pts',(4.90660088519391,0.185888877718945,4.59084243889714));
#30726=CARTESIAN_POINT('Ctrl Pts',(4.93045880322533,-0.119937101199393,
4.60767141961541));
#30727=CARTESIAN_POINT('Ctrl Pts',(4.95431672125674,-0.396435191853442,
4.47590818560059));
#30728=CARTESIAN_POINT('Ctrl Pts',(4.97817463928816,-0.575994079421511,
4.22777243672773));
#30729=CARTESIAN_POINT('Ctrl Pts',(5.00203255731958,-0.614706724807315,
3.92394012267834));
#30730=CARTESIAN_POINT('Ctrl Pts',(5.025890475351,-0.503106831702736,3.63870652046354));
#30731=CARTESIAN_POINT('Ctrl Pts',(5.04974839338242,-0.268483613891896,
3.44181901543221));
#30732=CARTESIAN_POINT('Ctrl Pts',(5.07360631141384,0.0317911608623165,
3.38142196567243));
#30733=CARTESIAN_POINT('Ctrl Pts',(5.09746422944526,0.32429213081186,3.47228409503311));
#30734=CARTESIAN_POINT('Ctrl Pts',(5.12132214747667,0.537494841237617,3.69218713785082));
#30735=CARTESIAN_POINT('Ctrl Pts',(5.1451800655081,0.619265421915264,3.98735881011802));
#30736=CARTESIAN_POINT('Ctrl Pts',(5.16903798353952,0.549608738483219,4.28562159765047));
#30737=CARTESIAN_POINT('Ctrl Pts',(5.19289590157094,0.34555774745058,4.51404212438126));
#30738=CARTESIAN_POINT('Ctrl Pts',(5.21675381960235,0.0570084743622218,
4.61676534947452));
#30739=CARTESIAN_POINT('Ctrl Pts',(5.24061173763377,-0.245480923587363,
4.56867264627043));
#30740=CARTESIAN_POINT('Ctrl Pts',(5.26446965566519,-0.487943548953736,
4.38152399072137));
#30741=CARTESIAN_POINT('Ctrl Pts',(5.28832757369661,-0.611090685285508,
4.10108232693608));
#30742=CARTESIAN_POINT('Ctrl Pts',(5.31218549172803,-0.584809503288917,
3.79592328078761));
#30743=CARTESIAN_POINT('Ctrl Pts',(5.33604340975945,-0.415526467847156,
3.5406665514248));
#30744=CARTESIAN_POINT('Ctrl Pts',(5.35990132779088,-0.144635892303038,
3.39772936223054));
#30745=CARTESIAN_POINT('Ctrl Pts',(5.38375924582228,0.161622098711782,3.40206374949372));
#30746=CARTESIAN_POINT('Ctrl Pts',(5.40761716385371,0.428359084093981,3.55260983746209));
#30747=CARTESIAN_POINT('Ctrl Pts',(5.43147508188512,0.590350605148055,3.81255500683439));
#30748=CARTESIAN_POINT('Ctrl Pts',(5.45533299991655,0.607985322415754,4.11833558293467));
#30749=CARTESIAN_POINT('Ctrl Pts',(5.47919091794796,0.476951067165249,4.39517988561105));
#30750=CARTESIAN_POINT('Ctrl Pts',(5.50304883597938,0.2292892841064,4.57539194177126));
#30751=CARTESIAN_POINT('Ctrl Pts',(5.5269067540108,-0.0744399746307492,
4.61490499480714));
#30752=CARTESIAN_POINT('Ctrl Pts',(5.55076467204222,-0.359966631867259,
4.5040570269359));
#30753=CARTESIAN_POINT('Ctrl Pts',(5.57462259007364,-0.55747164231658,4.26995338574299));
#30754=CARTESIAN_POINT('Ctrl Pts',(5.59848050810506,-0.618659650999605,
3.96983878834977));
#30755=CARTESIAN_POINT('Ctrl Pts',(5.62233842613648,-0.528568523057477,
3.67709942878664));
#30756=CARTESIAN_POINT('Ctrl Pts',(5.6461963441679,-0.309227993320144,3.46331805450751));
#30757=CARTESIAN_POINT('Ctrl Pts',(5.67005426219932,-0.0142727959960426,
3.38077003484781));
#30758=CARTESIAN_POINT('Ctrl Pts',(5.69391218023074,0.284172488697173,3.4496406091084));
#30759=CARTESIAN_POINT('Ctrl Pts',(5.71777009826216,0.513129859266986,3.65308904601577));
#30760=CARTESIAN_POINT('Ctrl Pts',(5.74162801629357,0.616613001744231,3.94136666067651));
#30761=CARTESIAN_POINT('Ctrl Pts',(5.765485934325,0.569317469330215,4.24398172424487));
#30762=CARTESIAN_POINT('Ctrl Pts',(5.78934385235641,0.382808307322586,4.48693660973462));
#30763=CARTESIAN_POINT('Ctrl Pts',(5.81320177038783,0.102692087527565,4.61082223133738));
#30764=CARTESIAN_POINT('Ctrl Pts',(5.83705968841925,-0.202535146533943,
4.58534517687525));
#30765=CARTESIAN_POINT('Ctrl Pts',(5.86091760645067,-0.458237017319611,
4.41673528603543));
#30766=CARTESIAN_POINT('Ctrl Pts',(5.88477552448209,-0.601887460912657,
4.14622225884759));
#30767=CARTESIAN_POINT('Ctrl Pts',(5.9086334425135,-0.598360014525416,3.83995392008642));
#30768=CARTESIAN_POINT('Ctrl Pts',(5.93249136054493,-0.448517265794504,
3.57282118150817));
#30769=CARTESIAN_POINT('Ctrl Pts',(5.95634927857635,-0.188999790056246,
3.41014534911766));
#30770=CARTESIAN_POINT('Ctrl Pts',(5.98020719660777,0.116733210556207,3.39170495376011));
#30771=CARTESIAN_POINT('Ctrl Pts',(6.00406511463918,0.393921897475357,3.52200944135141));
#30772=CARTESIAN_POINT('Ctrl Pts',(6.02792303267061,0.574785693380153,3.76919531120668));
#30773=CARTESIAN_POINT('Ctrl Pts',(6.05178095070201,0.61509921541814,4.07281983667942));
#30774=CARTESIAN_POINT('Ctrl Pts',(6.07563886873346,0.505003308517799,4.35863675364492));
#30775=CARTESIAN_POINT('Ctrl Pts',(6.09949678676485,0.27142206589204,4.55675943366228));
#30776=CARTESIAN_POINT('Ctrl Pts',(6.12335470479629,-0.0285325303540597,
4.61873507756083));
#30777=CARTESIAN_POINT('Ctrl Pts',(6.14721262282769,-0.321503980505702,
4.52942105023226));
#30778=CARTESIAN_POINT('Ctrl Pts',(6.17107054085913,-0.535870591003297,
4.31063422072759));
#30779=CARTESIAN_POINT('Ctrl Pts',(6.19492845889052,-0.619180264299368,
4.01591706164003));
#30780=CARTESIAN_POINT('Ctrl Pts',(6.21878637692196,-0.551125001039776,
3.71725450231754));
#30781=CARTESIAN_POINT('Ctrl Pts',(6.24264429495337,-0.348226295733882,
3.48783145534908));
#30782=CARTESIAN_POINT('Ctrl Pts',(6.2665022129848,-0.0603247367796791,
3.38345774569467));
#30783=CARTESIAN_POINT('Ctrl Pts',(6.29036013101621,0.242607149567705,3.43020375417728));
#30784=CARTESIAN_POINT('Ctrl Pts',(6.31421804904763,0.485688404846908,3.61560451082823));
#30785=CARTESIAN_POINT('Ctrl Pts',(6.33807596707905,0.61099356578022,3.89627130770405));
#30786=CARTESIAN_POINT('Ctrl Pts',(6.36193388511046,0.585080291527744,4.19994745529594));
#30787=CARTESIAN_POINT('Ctrl Pts',(6.3937444424857,0.363797450650833,4.54512657044717));
#30788=CARTESIAN_POINT('Ctrl Pts',(6.43350763920472,-0.178959141669374,
4.67939801199369));
#30789=CARTESIAN_POINT('Ctrl Pts',(6.48122347526757,-0.668951848353412,
4.21606826543601));
#30790=CARTESIAN_POINT('Ctrl Pts',(6.5289393113304,-0.543175254381078,3.55462676401443));
#30791=CARTESIAN_POINT('Ctrl Pts',(6.57665514739324,0.0806513803028556,
3.30201433154981));
#30792=CARTESIAN_POINT('Ctrl Pts',(6.62437098345608,0.630812951656228,3.69045991683978));
#30793=CARTESIAN_POINT('Ctrl Pts',(6.67208681951892,0.601478580142798,4.36311480674272));
#30794=CARTESIAN_POINT('Ctrl Pts',(6.71980265558175,0.0199087309838695,
4.70234020845997));
#30795=CARTESIAN_POINT('Ctrl Pts',(6.76751849164459,-0.580002689552455,
4.39658285339385));
#30796=CARTESIAN_POINT('Ctrl Pts',(6.81523432770743,-0.64725742864426,3.72664421308375));
#30797=CARTESIAN_POINT('Ctrl Pts',(6.86295016377027,-0.120142281411799,
3.30772876957018));
#30798=CARTESIAN_POINT('Ctrl Pts',(6.91066599983311,0.517310146858294,3.52453857056345));
#30799=CARTESIAN_POINT('Ctrl Pts',(6.95838183589594,0.679704059947864,4.17797090041396));
#30800=CARTESIAN_POINT('Ctrl Pts',(7.00609767195879,0.217917737520193,4.66797035296266));
#30801=CARTESIAN_POINT('Ctrl Pts',(7.05381350802161,-0.443987099894697,
4.54456206689342));
#30802=CARTESIAN_POINT('Ctrl Pts',(7.10152934408447,-0.698171061503544,
3.92107420680554));
#30803=CARTESIAN_POINT('Ctrl Pts',(7.14924518014729,-0.311214160204793,
3.3700650369752));
#30804=CARTESIAN_POINT('Ctrl Pts',(7.19696101621015,0.361535686685884,3.39753487888718));
#30805=CARTESIAN_POINT('Ctrl Pts',(7.24467685227297,0.702281647003851,3.97825768917858));
#30806=CARTESIAN_POINT('Ctrl Pts',(7.29239268833582,0.398111619195611,4.5789468099385));
#30807=CARTESIAN_POINT('Ctrl Pts',(7.34010852439865,-0.271650463017158,
4.64798016059173));
#30808=CARTESIAN_POINT('Ctrl Pts',(7.38782436046149,-0.691951729928866,
4.1219633626529));
#30809=CARTESIAN_POINT('Ctrl Pts',(7.43554019652432,-0.476823084268312,
3.48394573037578));
#30810=CARTESIAN_POINT('Ctrl Pts',(7.48325603258717,0.17617954081454,3.31982867534575));
#30811=CARTESIAN_POINT('Ctrl Pts',(7.53097186865001,0.667393780433987,3.78032341303133));
#30812=CARTESIAN_POINT('Ctrl Pts',(7.57868770471284,0.545730043505963,4.44255054095139));
#30813=CARTESIAN_POINT('Ctrl Pts',(7.62640354077568,-0.077085990144297,
4.69837669746149));
#30814=CARTESIAN_POINT('Ctrl Pts',(7.67411937683852,-0.629112772588521,
4.31287278685955));
#30815=CARTESIAN_POINT('Ctrl Pts',(7.72183521290136,-0.603415615998442,
3.64005298187887));
#30816=CARTESIAN_POINT('Ctrl Pts',(7.76955104896419,-0.0235926144000291,
3.29777806215626));
#30817=CARTESIAN_POINT('Ctrl Pts',(7.81726688502703,0.577895847971041,3.60036435301798));
#30818=CARTESIAN_POINT('Ctrl Pts',(7.86498272108987,0.648693661106154,4.26994220769392));
#30819=CARTESIAN_POINT('Ctrl Pts',(7.9126985571527,0.123786103798515,4.6916279794467));
#30820=CARTESIAN_POINT('Ctrl Pts',(7.96041439321555,-0.514796137313916,
4.47818113561083));
#30821=CARTESIAN_POINT('Ctrl Pts',(8.00813022927838,-0.680633164378164,
3.82561319718015));
#30822=CARTESIAN_POINT('Ctrl Pts',(8.05584606534123,-0.221434283704469,
3.33318734306526));
#30823=CARTESIAN_POINT('Ctrl Pts',(8.10356190140405,0.441111106898351,3.45310581204486));
#30824=CARTESIAN_POINT('Ctrl Pts',(8.1512777374669,0.698577380670183,4.07524562887252));
#30825=CARTESIAN_POINT('Ctrl Pts',(8.19899357352974,0.314529296777622,4.62828622690367));
#30826=CARTESIAN_POINT('Ctrl Pts',(8.24670940959258,-0.358355880000973,
4.60436191534297));
#30827=CARTESIAN_POINT('Ctrl Pts',(8.29442524565541,-0.70215733816079,4.02544275761943));
#30828=CARTESIAN_POINT('Ctrl Pts',(8.34214108171825,-0.401156908608127,
3.42315912408683));
#30829=CARTESIAN_POINT('Ctrl Pts',(8.3898569177811,0.268232082711808,3.35059734274305));
#30830=CARTESIAN_POINT('Ctrl Pts',(8.43757275384392,0.691299425196396,3.8743920139026));
#30831=CARTESIAN_POINT('Ctrl Pts',(8.48528858990677,0.479535868514212,4.51353443142269));
#30832=CARTESIAN_POINT('Ctrl Pts',(8.53300442596961,-0.172592854832336,
4.68109027882443));
#30833=CARTESIAN_POINT('Ctrl Pts',(8.58072026203244,-0.66622690390392,4.22319044326068));
#30834=CARTESIAN_POINT('Ctrl Pts',(8.62843609809529,-0.548054535901959,
3.56033138942427));
#30835=CARTESIAN_POINT('Ctrl Pts',(8.67615193415812,0.0734047453217555,
3.30122678585069));
#30836=CARTESIAN_POINT('Ctrl Pts',(8.72386777022095,0.627455319439314,3.68381637683837));
#30837=CARTESIAN_POINT('Ctrl Pts',(8.7715836062838,0.605304019074675,4.35676225408577));
#30838=CARTESIAN_POINT('Ctrl Pts',(8.81929944234663,0.0272927241942496,
4.70208786391332));
#30839=CARTESIAN_POINT('Ctrl Pts',(8.86701527840948,-0.575781899266294,
4.40267538529889));
#30840=CARTESIAN_POINT('Ctrl Pts',(8.9147311144723,-0.650107145087294,3.73347990440727));
#30841=CARTESIAN_POINT('Ctrl Pts',(8.96244695053515,-0.127428996390418,
3.30903392823725));
#30842=CARTESIAN_POINT('Ctrl Pts',(9.01016278659798,0.512269160438921,3.51911272764658));
#30843=CARTESIAN_POINT('Ctrl Pts',(9.05787862266082,0.681542664962993,4.17079770865984));
#30844=CARTESIAN_POINT('Ctrl Pts',(9.10559445872366,0.224945053369686,4.66563652575022));
#30845=CARTESIAN_POINT('Ctrl Pts',(9.1533102947865,-0.438223061957547,4.54921107910972));
#30846=CARTESIAN_POINT('Ctrl Pts',(9.20102613084934,-0.698964196560635,
3.92843664782408));
#30847=CARTESIAN_POINT('Ctrl Pts',(9.24874196691217,-0.317835754515511,
3.3733799439853));
#30848=CARTESIAN_POINT('Ctrl Pts',(9.29645780297501,0.355166151432911,3.39375807937372));
#30849=CARTESIAN_POINT('Ctrl Pts',(9.34417363903786,0.702013515586798,3.97085749870423));
#30850=CARTESIAN_POINT('Ctrl Pts',(9.39188947510068,0.404191066510942,4.57471892538967));
#30851=CARTESIAN_POINT('Ctrl Pts',(9.43960531116354,-0.264806258220881,
4.65080711970243));
#30852=CARTESIAN_POINT('Ctrl Pts',(9.48732114722635,-0.690627921460452,
4.12924912203773));
#30853=CARTESIAN_POINT('Ctrl Pts',(9.53503698328922,-0.482235337746388,
3.48899966685243));
#30854=CARTESIAN_POINT('Ctrl Pts',(9.58275281935202,0.169001376764621,3.31800968034731));
#30855=CARTESIAN_POINT('Ctrl Pts',(9.63046865541491,0.665041526572246,3.77330189814918));
#30856=CARTESIAN_POINT('Ctrl Pts',(9.6781844914777,0.550363809549371,4.43677447107931));
#30857=CARTESIAN_POINT('Ctrl Pts',(9.72590032754056,-0.0697214622184181,
4.69915032657822));
#30858=CARTESIAN_POINT('Ctrl Pts',(9.7736161636034,-0.625780442428439,4.31948567936979));
#30859=CARTESIAN_POINT('Ctrl Pts',(9.82133199966623,-0.607175613486645,
3.64643241687702));
#30860=CARTESIAN_POINT('Ctrl Pts',(9.86904783572907,-0.030992076082374,
3.29806570630264));
#30861=CARTESIAN_POINT('Ctrl Pts',(9.91676367179191,0.573651961662729,3.59429605827795));
#30862=CARTESIAN_POINT('Ctrl Pts',(9.96447950785474,0.651502576242943,4.26309058249416));
#30863=CARTESIAN_POINT('Ctrl Pts',(10.0121953439176,0.131068350403577,4.69028497663703));
#30864=CARTESIAN_POINT('Ctrl Pts',(10.0599111799804,-0.50972795835719,4.48358005533451));
#30865=CARTESIAN_POINT('Ctrl Pts',(10.1076270160433,-0.682433239785766,
3.83279612838271));
#30866=CARTESIAN_POINT('Ctrl Pts',(10.1553428521061,-0.228449576533966,
3.33555808949935));
#30867=CARTESIAN_POINT('Ctrl Pts',(10.2030586881689,0.435322847997542,3.44848728078164));
#30868=CARTESIAN_POINT('Ctrl Pts',(10.2507745242318,0.699331602909907,4.06787908823615));
#30869=CARTESIAN_POINT('Ctrl Pts',(10.2984903602946,0.321133386270249,4.62493648450936));
#30870=CARTESIAN_POINT('Ctrl Pts',(10.3462061963575,-0.351966560253669,
4.60810509117381));
#30871=CARTESIAN_POINT('Ctrl Pts',(10.3939220324203,-0.701850198794989,
4.03284143571381));
#30872=CARTESIAN_POINT('Ctrl Pts',(10.4416378684831,-0.407214000429435,
3.42741898450738));
#30873=CARTESIAN_POINT('Ctrl Pts',(10.489353704546,0.261373080323254,3.34780649011919));
#30874=CARTESIAN_POINT('Ctrl Pts',(10.5370695406088,0.689937239673316,3.86711333114163));
#30875=CARTESIAN_POINT('Ctrl Pts',(10.5847853766716,0.484921415782374,4.50845204490092));
#30876=CARTESIAN_POINT('Ctrl Pts',(10.6325012127345,-0.165405205696588,
4.68287142228737));
#30877=CARTESIAN_POINT('Ctrl Pts',(10.6802170487973,-0.66383768169814,4.23019946525991));
#30878=CARTESIAN_POINT('Ctrl Pts',(10.7279328848602,-0.552657800140614,
3.5661317972102));
#30879=CARTESIAN_POINT('Ctrl Pts',(10.775648720923,0.0660362430193439,3.30049197570278));
#30880=CARTESIAN_POINT('Ctrl Pts',(10.8233645569858,0.624088188116435,3.67722113622194));
#30881=CARTESIAN_POINT('Ctrl Pts',(10.8710803930487,0.609030347235101,4.3503630939397));
#30882=CARTESIAN_POINT('Ctrl Pts',(10.9187962291115,0.0346905673513346,
4.70176123146349));
#30883=CARTESIAN_POINT('Ctrl Pts',(10.9665120651743,-0.57150609431415,4.40872123214985));
#30884=CARTESIAN_POINT('Ctrl Pts',(11.0142279012372,-0.65287991581936,3.74034623636848));
#30885=CARTESIAN_POINT('Ctrl Pts',(11.0619437373,-0.134704064778877,3.31041528701663));
#30886=CARTESIAN_POINT('Ctrl Pts',(11.1096595733629,0.507172601636502,3.51374059022208));
#30887=CARTESIAN_POINT('Ctrl Pts',(11.1573754094257,0.68330486411552,4.16360539148934));
#30888=CARTESIAN_POINT('Ctrl Pts',(11.2050912454885,0.231947755880478,4.66322884435941));
#30889=CARTESIAN_POINT('Ctrl Pts',(11.2528070815514,-0.432410545554582,
4.55379904436673));
#30890=CARTESIAN_POINT('Ctrl Pts',(11.3005229176142,-0.699679589515398,
3.93580706063847));
#30891=CARTESIAN_POINT('Ctrl Pts',(11.348238753677,-0.324422100469907,3.37676444086124));
#30892=CARTESIAN_POINT('Ctrl Pts',(11.3959545897399,0.348757195312759,3.39004862475285));
#30893=CARTESIAN_POINT('Ctrl Pts',(11.4436704258027,0.701667392320496,3.9634605418422));
#30894=CARTESIAN_POINT('Ctrl Pts',(11.4913862618656,0.410225626419724,4.57042720558968));
#30895=CARTESIAN_POINT('Ctrl Pts',(11.5391020979284,-0.257932644354891,
4.65356178929341));
#30896=CARTESIAN_POINT('Ctrl Pts',(11.5868179339912,-0.689227399014534,
4.13652052554825));
#30897=CARTESIAN_POINT('Ctrl Pts',(11.6345337700541,-0.487594028032435,
3.49411036255383));
#30898=CARTESIAN_POINT('Ctrl Pts',(11.6822496061169,0.161804441490335,3.31626643773886));
#30899=CARTESIAN_POINT('Ctrl Pts',(11.7299654421798,0.662615402711184,3.76630556374144));
#30900=CARTESIAN_POINT('Ctrl Pts',(11.7776812782426,0.554936443973853,4.43094988641136));
#30901=CARTESIAN_POINT('Ctrl Pts',(11.8253971143054,-0.062349190059417,
4.69984629737339));
#30902=CARTESIAN_POINT('Ctrl Pts',(11.8731129503683,-0.622378603495518,
4.32606308493799));
#30903=CARTESIAN_POINT('Ctrl Pts',(11.9208287864311,-0.610868168815925,
3.65285112447858));
#30904=CARTESIAN_POINT('Ctrl Pts',(11.9685446224939,-0.0383880952977111,
3.29843131798253));
#30905=CARTESIAN_POINT('Ctrl Pts',(12.0162604585568,0.569344356809164,3.58827282720487));
#30906=CARTESIAN_POINT('Ctrl Pts',(12.0639762946196,0.654239125569198,4.25620973444184));
#30907=CARTESIAN_POINT('Ctrl Pts',(12.1116921306825,0.138336038556134,4.68886530024737));
#30908=CARTESIAN_POINT('Ctrl Pts',(12.1594079667453,-0.50460316123658,4.48892526128066));
#30909=CARTESIAN_POINT('Ctrl Pts',(12.2071238028081,-0.684157513748105,
3.83999763179777));
#30910=CARTESIAN_POINT('Ctrl Pts',(12.254839638871,-0.235439494268261,3.33800263898788));
#30911=CARTESIAN_POINT('Ctrl Pts',(12.3025554749338,0.429486235500398,3.44393000893412));
#30912=CARTESIAN_POINT('Ctrl Pts',(12.3502713109967,0.700008146713868,4.06050500791278));
#30913=CARTESIAN_POINT('Ctrl Pts',(12.3979871470595,0.327701805790174,4.62151732713591));
#30914=CARTESIAN_POINT('Ctrl Pts',(12.4457029831223,-0.345538145731053,
4.61178072157682));
#30915=CARTESIAN_POINT('Ctrl Pts',(12.4934188191852,-0.701465101239671,
4.04023646593735));
#30916=CARTESIAN_POINT('Ctrl Pts',(12.541134655248,-0.413225860851952,3.43174244451));
#30917=CARTESIAN_POINT('Ctrl Pts',(12.5888504913108,0.254485045853264,3.34508808005552));
#30918=CARTESIAN_POINT('Ctrl Pts',(12.6365663273737,0.688498419195676,3.85984940880123));
#30919=CARTESIAN_POINT('Ctrl Pts',(12.6842821634365,0.490253100280801,4.50331318193882));
#30920=CARTESIAN_POINT('Ctrl Pts',(12.7319979994994,-0.158199184135511,
4.68457671563321));
#30921=CARTESIAN_POINT('Ctrl Pts',(12.7797138355622,-0.661374723552845,
4.23718291779492));
#30922=CARTESIAN_POINT('Ctrl Pts',(12.827429671625,-0.557199677773407,3.57198039701723));
#30923=CARTESIAN_POINT('Ctrl Pts',(12.8751455076879,0.058660405724426,3.29983486358678));
#30924=CARTESIAN_POINT('Ctrl Pts',(12.9228613437507,0.62065173603916,3.67066174834999));
#30925=CARTESIAN_POINT('Ctrl Pts',(12.9705771798135,0.612689027194643,4.34392501712378));
#30926=CARTESIAN_POINT('Ctrl Pts',(13.0182930158764,0.0420845572448178,
4.7013566507062));
#30927=CARTESIAN_POINT('Ctrl Pts',(13.0660088519392,-0.567166809177069,
4.4147216801859));
#30928=CARTESIAN_POINT('Ctrl Pts',(13.1137246880021,-0.655580167748548,
3.74724140943759));
#30929=CARTESIAN_POINT('Ctrl Pts',(13.1614405240649,-0.141964170879043,
3.31187324159358));
#30930=CARTESIAN_POINT('Ctrl Pts',(13.2091563601277,0.502019708508231,3.50842246418533));
#30931=CARTESIAN_POINT('Ctrl Pts',(13.2568721961906,0.684991165006287,4.15639490180834));
#30932=CARTESIAN_POINT('Ctrl Pts',(13.3045880322534,0.238924694735218,4.66074749465585));
#30933=CARTESIAN_POINT('Ctrl Pts',(13.3523038683163,-0.426549999040181,
4.55832549625387));
#30934=CARTESIAN_POINT('Ctrl Pts',(13.4000197043791,-0.700317265381609,
3.94318460369993));
#30935=CARTESIAN_POINT('Ctrl Pts',(13.4477355404419,-0.330972411156884,
3.38021816378559));
#30936=CARTESIAN_POINT('Ctrl Pts',(13.4954513765048,0.342309500898352,3.3864069206363));
#30937=CARTESIAN_POINT('Ctrl Pts',(13.5431672125676,0.70124333116994,3.95606764360979));
#30938=CARTESIAN_POINT('Ctrl Pts',(13.5908830486304,0.416214620412595,4.5660721254426));
#30939=CARTESIAN_POINT('Ctrl Pts',(13.6385988846933,-0.251030380554765,
4.65624386434224));
#30940=CARTESIAN_POINT('Ctrl Pts',(13.6863147207561,-0.687750320459788,
4.14377676500662));
#30941=CARTESIAN_POINT('Ctrl Pts',(13.734030556819,-0.492898558687668,3.49927725007553));
#30942=CARTESIAN_POINT('Ctrl Pts',(13.7817463928818,0.15458953374652,3.31459914100992));
#30943=CARTESIAN_POINT('Ctrl Pts',(13.8294622289446,0.660115678675556,3.75933518700271));
#30944=CARTESIAN_POINT('Ctrl Pts',(13.8771780650075,0.559447438691528,4.42507743387505));
#30945=CARTESIAN_POINT('Ctrl Pts',(13.9248939010703,-0.0549699924482557,
4.7004645325629));
#30946=CARTESIAN_POINT('Ctrl Pts',(13.9726097371331,-0.61890763370075,4.33260427296601));
#30947=CARTESIAN_POINT('Ctrl Pts',(14.020325573196,-0.614492871807821,3.65930839172987));
#30948=CARTESIAN_POINT('Ctrl Pts',(14.0680414092588,-0.0457798505455885,
3.29887485658241));
#30949=CARTESIAN_POINT('Ctrl Pts',(14.1157572453217,0.564973511886205,3.58229532883235));
#30950=CARTESIAN_POINT('Ctrl Pts',(14.1634730813845,0.656903005118004,4.24930042782804));
#30951=CARTESIAN_POINT('Ctrl Pts',(14.2111889174473,0.145588360997982,4.6873691079691));
#30952=CARTESIAN_POINT('Ctrl Pts',(14.2589047535102,-0.499422315191365,
4.49421615972892));
#30953=CARTESIAN_POINT('Ctrl Pts',(14.306620589573,-0.685805794740406,3.8472169075166));
#30954=CARTESIAN_POINT('Ctrl Pts',(14.3543364256359,-0.242403260500786,
3.34052072000184));
#30955=CARTESIAN_POINT('Ctrl Pts',(14.4020522616987,0.423601917710294,3.43943450270243));
#30956=CARTESIAN_POINT('Ctrl Pts',(14.4497680977615,0.700606936934704,4.05312420698026));
#30957=CARTESIAN_POINT('Ctrl Pts',(14.4974839338244,0.334233825748585,4.61802913456711));
#30958=CARTESIAN_POINT('Ctrl Pts',(14.5451997698872,-0.339071350470923,
4.61538839828042));
#30959=CARTESIAN_POINT('Ctrl Pts',(14.59291560595,-0.701002088269634,4.04762702688518));
#30960=CARTESIAN_POINT('Ctrl Pts',(14.6406314420129,-0.419191822106764,
3.43612902386528));
#30961=CARTESIAN_POINT('Ctrl Pts',(14.6883472780757,0.24756874439201,3.34244241450009));
#30962=CARTESIAN_POINT('Ctrl Pts',(14.7360631141386,0.686983123580828,3.85260105372344));
#30963=CARTESIAN_POINT('Ctrl Pts',(14.7837789502014,0.495530329791292,4.49811841333687));
#30964=CARTESIAN_POINT('Ctrl Pts',(14.8314947862642,-0.150975590559777,
4.68620596944608));
#30965=CARTESIAN_POINT('Ctrl Pts',(14.8792106223271,-0.658838303041738,
4.24414002517693));
#30966=CARTESIAN_POINT('Ctrl Pts',(14.9269264583899,-0.561679664310124,
3.57787653921065));
#30967=CARTESIAN_POINT('Ctrl Pts',(14.9746422944528,0.0512780527100071,
3.29925552249156));
#30968=CARTESIAN_POINT('Ctrl Pts',(15.0223581305156,0.617146344912281,3.6641389418082));
#30969=CARTESIAN_POINT('Ctrl Pts',(15.0700739665784,0.616279652564493,4.337448738749));
#30970=CARTESIAN_POINT('Ctrl Pts',(15.1177898026413,0.0494738725853903,
4.70087416658037));
#30971=CARTESIAN_POINT('Ctrl Pts',(15.1655056387041,-0.562764525842253,
4.42067606290572));
#30972=CARTESIAN_POINT('Ctrl Pts',(15.2132214747669,-0.658207600943685,
3.75416465773151));
#30973=CARTESIAN_POINT('Ctrl Pts',(15.2609373108298,-0.14920850827279,3.31340763002542));
#30974=CARTESIAN_POINT('Ctrl Pts',(15.3086531468926,0.496811053413015,3.50315894024854));
#30975=CARTESIAN_POINT('Ctrl Pts',(15.3563689829554,0.686601380328997,4.14916704052379));
#30976=CARTESIAN_POINT('Ctrl Pts',(15.4040848190183,0.245875094968658,4.6581927522561));
#30977=CARTESIAN_POINT('Ctrl Pts',(15.4518006550811,-0.420642073376032,
4.56278993199436));
#30978=CARTESIAN_POINT('Ctrl Pts',(15.499516491144,-0.700877153329261,3.95056845754601));
#30979=CARTESIAN_POINT('Ctrl Pts',(15.5472323272068,-0.337485958999024,
3.3837407291352));
#30980=CARTESIAN_POINT('Ctrl Pts',(15.5949481632696,0.335823784368978,3.38283337152726));
#30981=CARTESIAN_POINT('Ctrl Pts',(15.6426639993325,0.70074137923783,3.94867962517506));
#30982=CARTESIAN_POINT('Ctrl Pts',(15.6903798353953,0.422157383260532,4.56165416869007));
#30983=CARTESIAN_POINT('Ctrl Pts',(15.7380956714582,-0.244100233491204,
4.65885304693675));
#30984=CARTESIAN_POINT('Ctrl Pts',(15.785811507521,-0.686196849863089,4.15101703442422));
#30985=CARTESIAN_POINT('Ctrl Pts',(15.8335273435838,-0.498148340509996,
3.50449975550414));
#30986=CARTESIAN_POINT('Ctrl Pts',(15.8812431796467,0.147357454930898,3.3130079753559));
#30987=CARTESIAN_POINT('Ctrl Pts',(15.9289590157095,0.657542632122849,3.75239154216938));
#30988=CARTESIAN_POINT('Ctrl Pts',(15.9766748517723,0.563896292642505,4.41915776575455));
#30989=CARTESIAN_POINT('Ctrl Pts',(16.0243906878352,-0.0475846890311933,
4.70100496347609));
#30990=CARTESIAN_POINT('Ctrl Pts',(16.072106523898,-0.615367918582998,4.33910851688972));
#30991=CARTESIAN_POINT('Ctrl Pts',(16.1198223599609,-0.618049319847516,
3.66580350138828));
#30992=CARTESIAN_POINT('Ctrl Pts',(16.1675381960237,-0.0531665207849041,
3.29939627283611));
#30993=CARTESIAN_POINT('Ctrl Pts',(16.2152540320865,0.560539912386559,3.57636422711252));
#30994=CARTESIAN_POINT('Ctrl Pts',(16.2629698681494,0.659493918998266,4.24236343010572));
#30995=CARTESIAN_POINT('Ctrl Pts',(16.3106857042122,0.152824512175573,4.68579656599215));
#30996=CARTESIAN_POINT('Ctrl Pts',(16.358401540275,-0.494185995685336,4.49945216299141));
#30997=CARTESIAN_POINT('Ctrl Pts',(16.4061173763379,-0.687377899679438,
3.85445315365633));
#30998=CARTESIAN_POINT('Ctrl Pts',(16.4538332124007,-0.249340101729437,
3.34311205284473));
#30999=CARTESIAN_POINT('Ctrl Pts',(16.5015490484636,0.417670548229327,3.43500126142608));
#31000=CARTESIAN_POINT('Ctrl Pts',(16.5492648845264,0.701127907061643,4.04573750526291));
#31001=CARTESIAN_POINT('Ctrl Pts',(16.5969807205892,0.340728720599694,4.61447229425484));
#31002=CARTESIAN_POINT('Ctrl Pts',(16.6446965566521,-0.3325668927742,4.61892772056098));
#31003=CARTESIAN_POINT('Ctrl Pts',(16.6924123927149,-0.700461211314163,
4.05501229764889));
#31004=CARTESIAN_POINT('Ctrl Pts',(16.7401282287777,-0.425111221523205,
3.4405782353328));
#31005=CARTESIAN_POINT('Ctrl Pts',(16.7878440648406,0.240624944169445,3.3398697873209));
#31006=CARTESIAN_POINT('Ctrl Pts',(16.8355599009034,0.685391521140609,3.84536907102113));
#31007=CARTESIAN_POINT('Ctrl Pts',(16.8832757369663,0.500752518144239,4.49286831610534));
#31008=CARTESIAN_POINT('Ctrl Pts',(16.9309915730291,-0.143735227331884,
4.68775900275617));
#31009=CARTESIAN_POINT('Ctrl Pts',(16.978707409092,-0.656228701898373,4.25107001464348));
#31010=CARTESIAN_POINT('Ctrl Pts',(17.0264232451548,-0.566097262135119,
3.58381956887496));
#31011=CARTESIAN_POINT('Ctrl Pts',(17.0741390812176,0.0438900039728252,
3.29875401676759));
#31012=CARTESIAN_POINT('Ctrl Pts',(17.1218549172805,0.613572404098014,3.65765344111895));
#31013=CARTESIAN_POINT('Ctrl Pts',(17.1695707533433,0.619801824515016,4.33093497816967));
#31014=CARTESIAN_POINT('Ctrl Pts',(17.2172865894061,0.0568576926029748,
4.70031383267802));
#31015=CARTESIAN_POINT('Ctrl Pts',(17.265002425469,-0.558299733294432,4.42658371892475));
#31016=CARTESIAN_POINT('Ctrl Pts',(17.3127182615318,-0.66076192356197,3.76111521224867));
#31017=CARTESIAN_POINT('Ctrl Pts',(17.3604340975947,-0.156436272293483,
3.31501828187956));
#31018=CARTESIAN_POINT('Ctrl Pts',(17.4081499336575,0.491547214903555,3.49795060305896));
#31019=CARTESIAN_POINT('Ctrl Pts',(17.4558657697204,0.688135331228569,4.14192261047223));
#31020=CARTESIAN_POINT('Ctrl Pts',(17.5035816057831,0.252798184563325,4.65556490092881));
#31021=CARTESIAN_POINT('Ctrl Pts',(17.551297441846,-0.414687424786488,4.56719185569987));
#31022=CARTESIAN_POINT('Ctrl Pts',(17.5990132779088,-0.701359191168653,
3.95795780201324));
#31023=CARTESIAN_POINT('Ctrl Pts',(17.6467291139717,-0.343962020502345,
3.38733174564023));
#31024=CARTESIAN_POINT('Ctrl Pts',(17.6944449500345,0.329300766127249,3.37932837435862));
#31025=CARTESIAN_POINT('Ctrl Pts',(17.7421607860974,0.700161592278611,3.94129730716402));
#31026=CARTESIAN_POINT('Ctrl Pts',(17.7898766221602,0.428053254869629,4.55717382605774));
#31027=CARTESIAN_POINT('Ctrl Pts',(17.837592458223,-0.23714297293205,4.66138904726133));
#31028=CARTESIAN_POINT('Ctrl Pts',(17.8853082942859,-0.684567159776581,
4.15824052958626));
#31029=CARTESIAN_POINT('Ctrl Pts',(17.9330241303487,-0.503342790378573,
3.50977729874859));
#31030=CARTESIAN_POINT('Ctrl Pts',(17.9807399664116,0.140109008348428,3.31149311751593));
#31031=CARTESIAN_POINT('Ctrl Pts',(18.0284558024744,0.654896548854854,3.7454754005085));
#31032=CARTESIAN_POINT('Ctrl Pts',(18.0761716385372,0.568282511669218,4.41319153957849));
#31033=CARTESIAN_POINT('Ctrl Pts',(18.1238874746001,-0.040194100132671,
4.70146753008449));
#31034=CARTESIAN_POINT('Ctrl Pts',(18.1716033106629,-0.611759851316993,
4.34557509424858));
#31035=CARTESIAN_POINT('Ctrl Pts',(18.2193191467258,-0.621537117901666,
3.67233573200791));
#31036=CARTESIAN_POINT('Ctrl Pts',(18.2670349827885,-0.0605472855394143,
3.29999550882718));
#31037=CARTESIAN_POINT('Ctrl Pts',(18.3147508188514,0.556044050773433,3.57048018084402));
#31038=CARTESIAN_POINT('Ctrl Pts',(18.3624666549143,0.662011579423562,4.23539951180373));
#31039=CARTESIAN_POINT('Ctrl Pts',(18.4101824909771,0.160043688331546,4.684147848987));
#31040=CARTESIAN_POINT('Ctrl Pts',(18.4578983270399,-0.488894784343999,
4.50463268947774));
#31041=CARTESIAN_POINT('Ctrl Pts',(18.5056141631028,-0.68887365394326,3.86170556644909));
#31042=CARTESIAN_POINT('Ctrl Pts',(18.5533299991656,-0.256249247442801,
3.34577634968359));
#31043=CARTESIAN_POINT('Ctrl Pts',(18.6010458352284,0.41169278588589,3.4306307775285));
#31044=CARTESIAN_POINT('Ctrl Pts',(18.6487616712913,0.701570999227752,4.03834572324048));
#31045=CARTESIAN_POINT('Ctrl Pts',(18.6964775073541,0.347185768921481,4.6108472012761));
#31046=CARTESIAN_POINT('Ctrl Pts',(18.744193343417,-0.326025495125306,4.62239829528727));
#31047=CARTESIAN_POINT('Ctrl Pts',(18.7919091794798,-0.699842530451103,
4.06239145790787));
#31048=CARTESIAN_POINT('Ctrl Pts',(18.8396250155426,-0.430983401602837,
3.44508958471478));
#31049=CARTESIAN_POINT('Ctrl Pts',(18.8873408516055,0.233654416470602,3.33737048427408));
#31050=CARTESIAN_POINT('Ctrl Pts',(18.9350566876683,0.683723788661416,3.83815426398688));
#31051=CARTESIAN_POINT('Ctrl Pts',(18.9827725237312,0.505919085286118,4.48756347340344));
#31052=CARTESIAN_POINT('Ctrl Pts',(19.030488359794,-0.136478898681533,4.68923564305365));
#31053=CARTESIAN_POINT('Ctrl Pts',(19.0782041958568,-0.653546209976322,
4.2579721164561));
#31054=CARTESIAN_POINT('Ctrl Pts',(19.1259200319197,-0.570451980578726,
3.58980882586423));
#31055=CARTESIAN_POINT('Ctrl Pts',(19.1736358679825,0.0364970801727598,
3.29833040216201));
#31056=CARTESIAN_POINT('Ctrl Pts',(19.2213517040453,0.609930310515188,3.65120596658116));
#31057=CARTESIAN_POINT('Ctrl Pts',(19.2690675401082,0.623255151928734,4.32438445905389));
#31058=CARTESIAN_POINT('Ctrl Pts',(19.316783376171,0.0642351969327414,4.69967571095415));
#31059=CARTESIAN_POINT('Ctrl Pts',(19.3644992122339,-0.553772927074266,
4.43244399258532));
#31060=CARTESIAN_POINT('Ctrl Pts',(19.4122150482967,-0.663242852612724,
3.76809229994096));
#31061=CARTESIAN_POINT('Ctrl Pts',(19.4599308843595,-0.163646658734412,
3.3167050201661));
#31062=CARTESIAN_POINT('Ctrl Pts',(19.5076467204224,0.486228775054438,3.49279802752061));
#31063=CARTESIAN_POINT('Ctrl Pts',(19.5553625564852,0.689592852244711,4.13466242315333));
#31064=CARTESIAN_POINT('Ctrl Pts',(19.6030783925481,0.259693185238344,4.65286421968052));
#31065=CARTESIAN_POINT('Ctrl Pts',(19.6507942286109,-0.408686697131164,
4.57153080275077));
#31066=CARTESIAN_POINT('Ctrl Pts',(19.6985100646738,-0.701763358503738,
3.96535177039745));
#31067=CARTESIAN_POINT('Ctrl Pts',(19.7462259007365,-0.350399813749482,
3.39099090115443));
#31068=CARTESIAN_POINT('Ctrl Pts',(19.7939417367994,0.322741052541778,3.37589215469092));
#31069=CARTESIAN_POINT('Ctrl Pts',(19.8416575728622,0.699504257835039,3.93392181877779));
#31070=CARTESIAN_POINT('Ctrl Pts',(19.8893734089251,0.433901159015506,4.55263101135276));
#31071=CARTESIAN_POINT('Ctrl Pts',(19.9370892449879,-0.23015857608315,4.663852686053));
#31072=CARTESIAN_POINT('Ctrl Pts',(19.9848050810507,-0.682862933423436,
4.16544436654047));
#31073=CARTESIAN_POINT('Ctrl Pts',(20.0325209171136,-0.508478494849655,
3.51511322409123));
#31074=CARTESIAN_POINT('Ctrl Pts',(20.0802367531764,0.132839643288252,3.31004731418368));
#31075=CARTESIAN_POINT('Ctrl Pts',(20.1279525892393,0.652187835720725,3.73860154375571));
#31076=CARTESIAN_POINT('Ctrl Pts',(20.1756684253021,0.572586513039731,4.4071529569233));
#31077=CARTESIAN_POINT('Ctrl Pts',(20.2233842613649,-0.0327629883405684,
4.70190215105461));
#31078=CARTESIAN_POINT('Ctrl Pts',(20.2711000974278,-0.608151935097038,
4.35190888358257));
#31079=CARTESIAN_POINT('Ctrl Pts',(20.3188159334906,-0.624827148513498,
3.67908301574286));
#31080=CARTESIAN_POINT('Ctrl Pts',(20.3665317695535,-0.0681655280739813,
3.30033184185188));
#31081=CARTESIAN_POINT('Ctrl Pts',(20.4142476056163,0.551956769749184,3.56531418539817));
#31082=CARTESIAN_POINT('Ctrl Pts',(20.4540108023353,0.644905999548395,4.11665253813788));
#31083=CARTESIAN_POINT('Ctrl Pts',(20.4858213597105,0.416382673412033,4.45708139504444));
#31084=CARTESIAN_POINT('Ctrl Pts',(20.509679277742,0.148137151166912,4.60177085628536));
#31085=CARTESIAN_POINT('Ctrl Pts',(20.5335371957734,-0.159214575149101,
4.59858486262053));
#31086=CARTESIAN_POINT('Ctrl Pts',(20.5573951138048,-0.426074836374489,
4.44942877587387));
#31087=CARTESIAN_POINT('Ctrl Pts',(20.5812530318362,-0.589577924844292,
4.19016123618585));
#31088=CARTESIAN_POINT('Ctrl Pts',(20.6051109498677,-0.608473233900696,
3.88450759853215));
#31089=CARTESIAN_POINT('Ctrl Pts',(20.6289688678991,-0.478813304308425,
3.60703485797333));
#31090=CARTESIAN_POINT('Ctrl Pts',(20.6528267859305,-0.231947052182395,
3.42568465323223));
#31091=CARTESIAN_POINT('Ctrl Pts',(20.6766847039619,0.0715712039811096,
3.38475332414555));
#31092=CARTESIAN_POINT('Ctrl Pts',(20.7005426219933,0.357622970648114,3.49427550111266));
#31093=CARTESIAN_POINT('Ctrl Pts',(20.7244005400248,0.556207844932749,3.72745636179159));
#31094=CARTESIAN_POINT('Ctrl Pts',(20.7482584580561,0.618794460414918,4.02728407199912));
#31095=CARTESIAN_POINT('Ctrl Pts',(20.7721163760876,0.530063832205264,4.32043875618714));
#31096=CARTESIAN_POINT('Ctrl Pts',(20.7959742941189,0.311720881859749,4.53523813880796));
#31097=CARTESIAN_POINT('Ctrl Pts',(20.8198322121505,0.01715224242355,4.619156844639));
#31098=CARTESIAN_POINT('Ctrl Pts',(20.8436901301818,-0.281609823618225,
4.55167503361081));
#31099=CARTESIAN_POINT('Ctrl Pts',(20.8675480482133,-0.511511021444125,
4.34929354512778));
#31100=CARTESIAN_POINT('Ctrl Pts',(20.8914059662447,-0.616333626991818,
4.06150032559224));
#31101=CARTESIAN_POINT('Ctrl Pts',(20.9152638842761,-0.570445985619195,
3.75866857192897));
#31102=CARTESIAN_POINT('Ctrl Pts',(20.9391218023075,-0.385068702031786,
3.51484894167474));
#31103=CARTESIAN_POINT('Ctrl Pts',(20.9629797203389,-0.105531663562905,
3.38966195221662));
#31104=CARTESIAN_POINT('Ctrl Pts',(20.9868376383704,0.199810758127152,3.41371924506628));
#31105=CARTESIAN_POINT('Ctrl Pts',(21.0106955564018,0.456293997792742,3.58113815016051));
#31106=CARTESIAN_POINT('Ctrl Pts',(21.0345534744332,0.60120093052663,3.85098018832832));
#31107=CARTESIAN_POINT('Ctrl Pts',(21.0584113924646,0.599097856858477,4.15726162902184));
#31108=CARTESIAN_POINT('Ctrl Pts',(21.082269310496,0.450499039416452,4.42508831804098));
#31109=CARTESIAN_POINT('Ctrl Pts',(21.1061272285275,0.191740934787398,4.58896933394457));
#31110=CARTESIAN_POINT('Ctrl Pts',(21.1299851465589,-0.113903050943465,
4.60883130459215));
#31111=CARTESIAN_POINT('Ctrl Pts',(21.1538430645903,-0.391694638258801,
4.47981743698434));
#31112=CARTESIAN_POINT('Ctrl Pts',(21.1777009826217,-0.573706216867813,
4.23347513609622));
#31113=CARTESIAN_POINT('Ctrl Pts',(21.2015589006531,-0.615430998064313,
3.9300418046833));
#31114=CARTESIAN_POINT('Ctrl Pts',(21.2254168186846,-0.506666136201032,
3.64371515765586));
#31115=CARTESIAN_POINT('Ctrl Pts',(21.2492747367159,-0.27400760274365,3.44450985958179));
#31116=CARTESIAN_POINT('Ctrl Pts',(21.2731326547474,0.0256532534100022,
3.38113703208972));
#31117=CARTESIAN_POINT('Ctrl Pts',(21.2969905727788,0.319041190319967,3.46909305773936));
#31118=CARTESIAN_POINT('Ctrl Pts',(21.3208484908102,0.534414865691478,3.68687029238709));
#31119=CARTESIAN_POINT('Ctrl Pts',(21.3447064088416,0.619109549231529,3.98121627002784));
#31120=CARTESIAN_POINT('Ctrl Pts',(21.3685643268731,0.552415083779586,4.28015538130547));
#31121=CARTESIAN_POINT('Ctrl Pts',(21.3924222449044,0.350640082858436,4.51058887057447));
#31122=CARTESIAN_POINT('Ctrl Pts',(21.4162801629359,0.0631240304344945,
4.61616947282646));
#31123=CARTESIAN_POINT('Ctrl Pts',(21.4401380809673,-0.239827566894842,
4.57107985485291));
#31124=CARTESIAN_POINT('Ctrl Pts',(21.4639959989987,-0.484134791346583,
4.38634565646493));
#31125=CARTESIAN_POINT('Ctrl Pts',(21.4878539170302,-0.610057871747176,
4.10713942122688));
#31126=CARTESIAN_POINT('Ctrl Pts',(21.5117118350615,-0.586805184862796,
3.80173467907963));
#31127=CARTESIAN_POINT('Ctrl Pts',(21.535569753093,-0.420062646027161,3.5448112085363));
#31128=CARTESIAN_POINT('Ctrl Pts',(21.5594276711244,-0.150603347961132,
3.39919379659958));
#31129=CARTESIAN_POINT('Ctrl Pts',(21.5832855891558,0.155682571034224,3.40048986702667));
#31130=CARTESIAN_POINT('Ctrl Pts',(21.6071435071872,0.423899860703612,3.54838249529388));
#31131=CARTESIAN_POINT('Ctrl Pts',(21.6310014252187,0.588462087630599,3.80670790527556));
#31132=CARTESIAN_POINT('Ctrl Pts',(21.6548593432501,0.609129304746478,4.11229849758833));
#31133=CARTESIAN_POINT('Ctrl Pts',(21.6787172612815,0.480847814502724,4.39042904829107));
#31134=CARTESIAN_POINT('Ctrl Pts',(21.7025751793129,0.234985935581564,4.57308906161293));
#31135=CARTESIAN_POINT('Ctrl Pts',(21.7264330973443,-0.0683364054776661,
4.61561318873779));
#31136=CARTESIAN_POINT('Ctrl Pts',(21.7502910153758,-0.35494863395129,4.5076031222497));
#31137=CARTESIAN_POINT('Ctrl Pts',(21.7741489334072,-0.554766252817153,
4.2754702655401));
#31138=CARTESIAN_POINT('Ctrl Pts',(21.7980068514386,-0.618928411339905,
3.9759774252466));
#31139=CARTESIAN_POINT('Ctrl Pts',(21.82186476947,-0.531745714018629,3.68235875884208));
#31140=CARTESIAN_POINT('Ctrl Pts',(21.8457226875014,-0.314536705157368,
3.46641202827438));
#31141=CARTESIAN_POINT('Ctrl Pts',(21.8695806055329,-0.0204149040773093,
3.3809420914381));
#31142=CARTESIAN_POINT('Ctrl Pts',(21.8934385235643,0.278698897140474,3.44684867604406));
#31143=CARTESIAN_POINT('Ctrl Pts',(21.9172964415957,0.509663226401888,3.6480158268968));
#31144=CARTESIAN_POINT('Ctrl Pts',(21.9411543596271,0.616001013860485,3.93525269592965));
#31145=CARTESIAN_POINT('Ctrl Pts',(21.9650122776585,0.571709773899469,4.23832204448885));
#31146=CARTESIAN_POINT('Ctrl Pts',(21.98887019569,0.387619921158457,4.48311516140836));
#31147=CARTESIAN_POINT('Ctrl Pts',(22.0127281137213,0.108746439139576,4.60977346157076));
#31148=CARTESIAN_POINT('Ctrl Pts',(22.0365860317528,-0.196718509442517,
4.5873255404835));
#31149=CARTESIAN_POINT('Ctrl Pts',(22.0604439497842,-0.454080423961193,
4.42126052632156));
#31150=CARTESIAN_POINT('Ctrl Pts',(22.0843018678156,-0.600407305919173,
4.15218583856754));
#31151=CARTESIAN_POINT('Ctrl Pts',(22.1081597858471,-0.599918246812857,
3.84589756782496));
#31152=CARTESIAN_POINT('Ctrl Pts',(22.1320177038785,-0.452732834916613,
3.57729153941473));
#31153=CARTESIAN_POINT('Ctrl Pts',(22.1558756219099,-0.194841912687001,
3.41204924396571));
#31154=CARTESIAN_POINT('Ctrl Pts',(22.1797335399413,0.110693164578993,3.39057692382254));
#31155=CARTESIAN_POINT('Ctrl Pts',(22.2035914579728,0.389160747889314,3.51812514615901));
#31156=CARTESIAN_POINT('Ctrl Pts',(22.2274493760041,0.572467927805029,3.76350489626149));
#31157=CARTESIAN_POINT('Ctrl Pts',(22.2513072940356,0.615791105677536,4.06671414123586));
#31158=CARTESIAN_POINT('Ctrl Pts',(22.2751652120669,0.508536584364246,4.35360996140145));
#31159=CARTESIAN_POINT('Ctrl Pts',(22.2990231300984,0.276931015980992,4.55403851389998));
#31160=CARTESIAN_POINT('Ctrl Pts',(22.3228810481298,-0.0223917293827815,
4.61898955797298));
#31161=CARTESIAN_POINT('Ctrl Pts',(22.3467389661613,-0.31623908674035,4.53258079431836));
#31162=CARTESIAN_POINT('Ctrl Pts',(22.3705968841927,-0.532757373651304,
4.31594151899069));
#31163=CARTESIAN_POINT('Ctrl Pts',(22.3944548022241,-0.619001969851995,
4.02204593667267));
#31164=CARTESIAN_POINT('Ctrl Pts',(22.4183127202555,-0.553883724721699,
3.72275952141814));
#31165=CARTESIAN_POINT('Ctrl Pts',(22.4421706382869,-0.35332581843718,3.49126595675675));
#31166=CARTESIAN_POINT('Ctrl Pts',(22.4660285563184,-0.0663701307507445,
3.38417172009386));
#31167=CARTESIAN_POINT('Ctrl Pts',(22.4898864743497,0.236814872379406,3.42766427875767));
#31168=CARTESIAN_POINT('Ctrl Pts',(22.5137443923812,0.482092168510832,3.61110849992699));
#31169=CARTESIAN_POINT('Ctrl Pts',(22.5376023104126,0.609484835267769,3.88964730767638));
#31170=CARTESIAN_POINT('Ctrl Pts',(22.561460228444,0.587841786482003,4.19517031382209));
#31171=CARTESIAN_POINT('Ctrl Pts',(22.5853181464754,0.422455543015367,4.45296893898932));
#31172=CARTESIAN_POINT('Ctrl Pts',(22.6091760645069,0.153767157666155,4.60000417439789));
#31173=CARTESIAN_POINT('Ctrl Pts',(22.6330339825383,-0.152521006364708,
4.60032232020799));
#31174=CARTESIAN_POINT('Ctrl Pts',(22.6568919005697,-0.421514535902825,
4.45384478734481));
#31175=CARTESIAN_POINT('Ctrl Pts',(22.6807498186011,-0.587434568575047,
4.19639082134502));
#31176=CARTESIAN_POINT('Ctrl Pts',(22.7046077366325,-0.60971407867596,3.89091209973551));
#31177=CARTESIAN_POINT('Ctrl Pts',(22.728465654664,-0.482895786937606,3.61211183522625));
#31178=CARTESIAN_POINT('Ctrl Pts',(22.7523235726954,-0.23800784887647,3.4281541921173));
#31179=CARTESIAN_POINT('Ctrl Pts',(22.7761814907268,0.0651013135850054,
3.38404091701771));
#31180=CARTESIAN_POINT('Ctrl Pts',(22.8000394087582,0.352249768808992,3.49052260401466));
#31181=CARTESIAN_POINT('Ctrl Pts',(22.8238973267896,0.553345940411564,3.72163220123786));
#31182=CARTESIAN_POINT('Ctrl Pts',(22.8398026054772,0.597082876783669,3.92101540361374));
#31183=CARTESIAN_POINT('Ctrl Pts',(22.847755244821,0.593766187829899,4.01991291515446));
#31184=CARTESIAN_POINT('',(22.8,0.337479661717902,3.51106003648017));
#31185=CARTESIAN_POINT('Ctrl Pts',(22.8,0.337504360408405,3.51101527402275));
#31186=CARTESIAN_POINT('Ctrl Pts',(22.8,0.337610992569967,3.51114843896934));
#31187=CARTESIAN_POINT('Ctrl Pts',(22.8,0.337717562131928,3.51128164981369));
#31188=CARTESIAN_POINT('Ctrl Pts',(22.8,0.337824069051012,3.51141490653789));
#31189=CARTESIAN_POINT('Ctrl Pts',(22.8,0.354145371784291,3.53183539523119));
#31190=CARTESIAN_POINT('Ctrl Pts',(22.8,0.368999739942303,3.55333386321799));
#31191=CARTESIAN_POINT('Ctrl Pts',(22.8,0.382262544471458,3.57576050230915));
#31192=CARTESIAN_POINT('Ctrl Pts',(22.8,0.395177725624396,3.59759933027929));
#31193=CARTESIAN_POINT('Ctrl Pts',(22.8,0.406583379369087,3.62031953557487));
#31194=CARTESIAN_POINT('Ctrl Pts',(22.8,0.416319965152677,3.64376476659274));
#31195=CARTESIAN_POINT('Ctrl Pts',(22.8,0.420499854003763,3.65382973822867));
#31196=CARTESIAN_POINT('Ctrl Pts',(22.8,0.424371599987778,3.66402799385056));
#31197=CARTESIAN_POINT('Ctrl Pts',(22.8,0.42792023461967,3.67434527679585));
#31198=CARTESIAN_POINT('Ctrl Pts',(22.8,0.430015882150509,3.68043815216119));
#31199=CARTESIAN_POINT('Ctrl Pts',(22.8,0.431995626466768,3.68656321156818));
#31200=CARTESIAN_POINT('Ctrl Pts',(22.8,0.433857425300493,3.69271766785326));
#31201=CARTESIAN_POINT('Ctrl Pts',(22.8,0.440667704273582,3.71523007009016));
#31202=CARTESIAN_POINT('Ctrl Pts',(22.8,0.445903532435623,3.73813926926309));
#31203=CARTESIAN_POINT('Ctrl Pts',(22.8,0.449441836754149,3.76130640751661));
#31204=CARTESIAN_POINT('Ctrl Pts',(22.8,0.450038513826676,3.76521316594877));
#31205=CARTESIAN_POINT('Ctrl Pts',(22.8,0.450586822418701,3.76912718643627));
#31206=CARTESIAN_POINT('Ctrl Pts',(22.8,0.451086059471329,3.77304770583064));
#31207=CARTESIAN_POINT('Ctrl Pts',(22.8,0.453684096906641,3.79345015011803));
#31208=CARTESIAN_POINT('Ctrl Pts',(22.8,0.454954433743694,3.81403106227893));
#31209=CARTESIAN_POINT('Ctrl Pts',(22.8,0.45484641916779,3.83463783350426));
#31210=CARTESIAN_POINT('Ctrl Pts',(22.8,0.454808390965019,3.84189276616533));
#31211=CARTESIAN_POINT('Ctrl Pts',(22.8,0.454599381710613,3.84915061719132));
#31212=CARTESIAN_POINT('Ctrl Pts',(22.8,0.454216814112443,3.8564037154462));
#31213=CARTESIAN_POINT('Ctrl Pts',(22.8,0.453866695925276,3.86304160538904));
#31214=CARTESIAN_POINT('Ctrl Pts',(22.8,0.453371644107099,3.86966645154658));
#31215=CARTESIAN_POINT('Ctrl Pts',(22.8,0.452731182295137,3.87626933737115));
#31216=CARTESIAN_POINT('Ctrl Pts',(22.8,0.450713457978438,3.89707120727158));
#31217=CARTESIAN_POINT('Ctrl Pts',(22.8,0.447253508643,3.9176725514372));
#31218=CARTESIAN_POINT('Ctrl Pts',(22.8,0.442312061254715,3.9379035771693));
#31219=CARTESIAN_POINT('Ctrl Pts',(22.8,0.437564183511961,3.95734209977996));
#31220=CARTESIAN_POINT('Ctrl Pts',(22.8,0.431447509288203,3.97643919003209));
#31221=CARTESIAN_POINT('Ctrl Pts',(22.8,0.423915075143768,3.9949978423605));
#31222=CARTESIAN_POINT('Ctrl Pts',(22.8,0.421325190817866,4.00137888225459));
#31223=CARTESIAN_POINT('Ctrl Pts',(22.8,0.418567902041021,4.00769582483512));
#31224=CARTESIAN_POINT('Ctrl Pts',(22.8,0.415641328671541,4.01393920819689));
#31225=CARTESIAN_POINT('Ctrl Pts',(22.6211545887425,-1.51173456864708E-7,
4.59404872180247));
#31226=CARTESIAN_POINT('Ctrl Pts',(22.6251143866744,-0.0492822808754852,
4.59404929162283));
#31227=CARTESIAN_POINT('Ctrl Pts',(22.6290741846063,-0.0985642856931001,
4.58798571459226));
#31228=CARTESIAN_POINT('Ctrl Pts',(22.6330339825383,-0.14630523394925,4.57585637376244));
#31229=CARTESIAN_POINT('Ctrl Pts',(22.6409866218821,-0.242185516210759,
4.55149647592026));
#31230=CARTESIAN_POINT('Ctrl Pts',(22.6489392612259,-0.331850026056775,
4.50267063163255));
#31231=CARTESIAN_POINT('Ctrl Pts',(22.6568919005697,-0.404335619758509,
4.43534871515538));
#31232=CARTESIAN_POINT('Ctrl Pts',(22.6648445399135,-0.476821213460227,
4.36802679867822));
#31233=CARTESIAN_POINT('Ctrl Pts',(22.6727971792573,-0.532127891017642,
4.28220881001161));
#31234=CARTESIAN_POINT('Ctrl Pts',(22.6807498186011,-0.563494481479829,
4.18838669541007));
#31235=CARTESIAN_POINT('Ctrl Pts',(22.6887024579449,-0.594861071942019,
4.09456458080851));
#31236=CARTESIAN_POINT('Ctrl Pts',(22.6966550972887,-0.602287575308989,
3.99273834027202));
#31237=CARTESIAN_POINT('Ctrl Pts',(22.7046077366325,-0.584864445036083,
3.89535850925222));
#31238=CARTESIAN_POINT('Ctrl Pts',(22.7125603759763,-0.567441314763176,
3.79797867823242));
#31239=CARTESIAN_POINT('Ctrl Pts',(22.7205130153201,-0.525168550850394,
3.70504525672934));
#31240=CARTESIAN_POINT('Ctrl Pts',(22.7284656546639,-0.463217512550482,
3.62791893879298));
#31241=CARTESIAN_POINT('Ctrl Pts',(22.7364182940078,-0.401266474250563,
3.5507926208566));
#31242=CARTESIAN_POINT('Ctrl Pts',(22.7443709333516,-0.319637161563486,
3.48947340648693));
#31243=CARTESIAN_POINT('Ctrl Pts',(22.7523235726954,-0.228304311476372,
3.45146158678551));
#31244=CARTESIAN_POINT('Ctrl Pts',(22.7602762120392,-0.136971461389268,
3.41344976708409));
#31245=CARTESIAN_POINT('Ctrl Pts',(22.768228851383,-0.0359350739021178,
3.3987453420509));
#31246=CARTESIAN_POINT('Ctrl Pts',(22.7761814907268,0.062441195712126,3.40914007736714));
#31247=CARTESIAN_POINT('Ctrl Pts',(22.7841209938178,0.160654966376612,3.41951764255099));
#31248=CARTESIAN_POINT('Ctrl Pts',(22.7920604969089,0.256217399931083,3.45491151845628));
#31249=CARTESIAN_POINT('Ctrl Pts',(22.8,0.337504360408238,3.51101527402264));
#31250=CARTESIAN_POINT('Ctrl Pts',(4.,-0.219914231356244,4.35301468169996));
#31251=CARTESIAN_POINT('Ctrl Pts',(4.00793950309107,-0.278596966840389,
4.31645650682028));
#31252=CARTESIAN_POINT('Ctrl Pts',(4.02383164552594,-0.377405665439666,
4.21337674819164));
#31253=CARTESIAN_POINT('Ctrl Pts',(4.04767642730463,-0.433534992178268,
4.00656196868444));
#31254=CARTESIAN_POINT('Ctrl Pts',(4.07153434533603,-0.383670022685343,
3.79803920418254));
#31255=CARTESIAN_POINT('Ctrl Pts',(4.09539226336747,-0.239994733226421,
3.63889579340969));
#31256=CARTESIAN_POINT('Ctrl Pts',(4.11925018139887,-0.0376302499649443,
3.56805514133307));
#31257=CARTESIAN_POINT('Ctrl Pts',(4.1431080994303,0.173933765839147,3.60283521426327));
#31258=CARTESIAN_POINT('Ctrl Pts',(4.16696601746172,0.342967344134064,3.73473372141871));
#31259=CARTESIAN_POINT('Ctrl Pts',(4.19082393549313,0.428135478754777,3.93149662217858));
#31260=CARTESIAN_POINT('Ctrl Pts',(4.21468185352456,0.40861313688017,4.1450106963618));
#31261=CARTESIAN_POINT('Ctrl Pts',(4.23853977155597,0.289173588337559,4.32306558264197));
#31262=CARTESIAN_POINT('Ctrl Pts',(4.25811226835493,0.13317859508208,4.40432939198872));
#31263=CARTESIAN_POINT('Ctrl Pts',(4.26973212581007,0.0319512750557707,
4.41584666103033));
#31264=CARTESIAN_POINT('Ctrl Pts',(4.2733993439214,2.51014653359152E-6,
4.41583996132385));
#31265=CARTESIAN_POINT('Origin',(3.42660065607856,0.,4.));
#31266=CARTESIAN_POINT('Ctrl Pts',(4.,-0.219892372743211,3.64701365460636));
#31267=CARTESIAN_POINT('Ctrl Pts',(4.00795263934381,-0.161099076858729,
3.61038844940468));
#31268=CARTESIAN_POINT('Ctrl Pts',(4.02385791803142,-0.0249198690254346,
3.56711791692558));
#31269=CARTESIAN_POINT('Ctrl Pts',(4.04771583606284,0.185569069288609,3.60813812632505));
#31270=CARTESIAN_POINT('Ctrl Pts',(4.07157375409426,0.350624105231944,3.74494568050885));
#31271=CARTESIAN_POINT('Ctrl Pts',(4.09543167212568,0.429971014252744,3.94413788601839));
#31272=CARTESIAN_POINT('Ctrl Pts',(4.1192895901571,0.40416308778273,4.15698104289539));
#31273=CARTESIAN_POINT('Ctrl Pts',(4.14314750818851,0.279534313346206,4.3314427366163));
#31274=CARTESIAN_POINT('Ctrl Pts',(4.16225119682902,0.125004509401131,4.40624063703925));
#31275=CARTESIAN_POINT('Ctrl Pts',(4.1734022461257,0.0278694809177792,4.41585864517498));
#31276=CARTESIAN_POINT('Ctrl Pts',(4.17660065607858,5.88453344126799E-6,
4.41584444980552));
#31277=CARTESIAN_POINT('Ctrl Pts',(3.95224475517896,-0.314128184302177,
3.49573985500833));
#31278=CARTESIAN_POINT('Ctrl Pts',(3.96019739452277,-0.230138771413741,
3.44341876234755));
#31279=CARTESIAN_POINT('Ctrl Pts',(3.97610267321038,-0.0355993848822847,
3.38160445914153));
#31280=CARTESIAN_POINT('Ctrl Pts',(3.9999605912418,0.265095483172694,3.44020405374152));
#31281=CARTESIAN_POINT('Ctrl Pts',(4.02381850927322,0.500885556761892,3.63564106712445));
#31282=CARTESIAN_POINT('Ctrl Pts',(4.04767642730465,0.614236921112272,3.92019793948569));
#31283=CARTESIAN_POINT('Ctrl Pts',(4.07153434533605,0.577368897990231,4.22425593648149));
#31284=CARTESIAN_POINT('Ctrl Pts',(4.09539226336749,0.399329932212592,4.47348393104611));
#31285=CARTESIAN_POINT('Ctrl Pts',(4.11925018139889,0.123637843932736,4.60692867011962));
#31286=CARTESIAN_POINT('Ctrl Pts',(4.14310809943032,-0.182283847264271,
4.59196468982869));
#31287=CARTESIAN_POINT('Ctrl Pts',(4.16696601746173,-0.443633876576525,
4.43224822622665));
#31288=CARTESIAN_POINT('Ctrl Pts',(4.19082393549315,-0.596502436238336,
4.16683582239239));
#31289=CARTESIAN_POINT('Ctrl Pts',(4.21468185352458,-0.603510379797736,
3.86062723727387));
#31290=CARTESIAN_POINT('Ctrl Pts',(4.23853977155598,-0.462943343075553,
3.58849923641164));
#31291=CARTESIAN_POINT('Ctrl Pts',(4.26239768958742,-0.209174182705692,
3.41699430327496));
#31292=CARTESIAN_POINT('Ctrl Pts',(4.28625560761882,0.0957438341235747,
3.38805018506757));
#31293=CARTESIAN_POINT('Ctrl Pts',(4.31011352565025,0.377249837899377,3.50874444390425));
#31294=CARTESIAN_POINT('Ctrl Pts',(4.33397144368167,0.566508000142931,3.7495640793295));
#31295=CARTESIAN_POINT('Ctrl Pts',(4.35782936171309,0.617239514437223,4.05162211295782));
#31296=CARTESIAN_POINT('Ctrl Pts',(4.3816872797445,0.517039159770137,4.34105713706075));
#31297=CARTESIAN_POINT('Ctrl Pts',(4.40554519777592,0.290408643717306,4.54709439922074));
#31298=CARTESIAN_POINT('Ctrl Pts',(4.42940311580735,-0.00723469473045889,
4.61935217913086));
#31299=CARTESIAN_POINT('Ctrl Pts',(4.45326103383876,-0.303108954077165,
4.54016147994594));
#31300=CARTESIAN_POINT('Ctrl Pts',(4.47711895187019,-0.524864817190473,
4.3288865854667));
#31301=CARTESIAN_POINT('Ctrl Pts',(4.5009768699016,-0.618276935702851,4.03718996201469));
#31302=CARTESIAN_POINT('Ctrl Pts',(4.52483478793302,-0.560503501787052,
3.7363993798876));
#31303=CARTESIAN_POINT('Ctrl Pts',(4.54869270596444,-0.365671693940747,
3.50006632967672));
#31304=CARTESIAN_POINT('Ctrl Pts',(4.57255062399586,-0.0814231961944085,
3.38598067979976));
#31305=CARTESIAN_POINT('Ctrl Pts',(4.59640854202727,0.222735490926488,3.42203947925158));
#31306=CARTESIAN_POINT('Ctrl Pts',(4.6202664600587,0.472429283332598,3.59942536936051));
#31307=CARTESIAN_POINT('Ctrl Pts',(4.64412437809011,0.606601247243452,3.87476266809168));
#31308=CARTESIAN_POINT('Ctrl Pts',(4.66798229612153,0.592442682719785,4.18072390587243));
#31309=CARTESIAN_POINT('Ctrl Pts',(4.69184021415295,0.433415744455024,4.44249322584619));
#31310=CARTESIAN_POINT('Ctrl Pts',(4.71569813218437,0.168406850663934,4.59606089882753));
#31311=CARTESIAN_POINT('Ctrl Pts',(4.7395560502158,-0.1377821054254,4.60387544567241));
#31312=CARTESIAN_POINT('Ctrl Pts',(4.7634139682472,-0.410279583628813,4.46402599681362));
#31313=CARTESIAN_POINT('Ctrl Pts',(4.78727188627863,-0.582452527843622,
4.21070955191949));
#31314=CARTESIAN_POINT('Ctrl Pts',(4.81112980431005,-0.612199963312297,
3.9058688819681));
#31315=CARTESIAN_POINT('Ctrl Pts',(4.83498772234147,-0.492247831758966,
3.62404583445569));
#31316=CARTESIAN_POINT('Ctrl Pts',(4.85884564037289,-0.251927696778831,
3.4341538212047));
#31317=CARTESIAN_POINT('Ctrl Pts',(4.88270355840431,0.0499956224363984,
3.38262661200963));
#31318=CARTESIAN_POINT('Ctrl Pts',(4.90656147643572,0.339693650112522,3.48206401309162));
#31319=CARTESIAN_POINT('Ctrl Pts',(4.93041939446714,0.546327327266884,3.70815087126575));
#31320=CARTESIAN_POINT('Ctrl Pts',(4.95427731249857,0.619369091246891,4.00560279122603));
#31321=CARTESIAN_POINT('Ctrl Pts',(4.97813523052998,0.540958241141728,4.3016846761146));
#31322=CARTESIAN_POINT('Ctrl Pts',(5.00199314856141,0.330268365670778,4.52399643996756));
#31323=CARTESIAN_POINT('Ctrl Pts',(5.02585106659282,0.0388188784636707,
4.61817680087201));
#31324=CARTESIAN_POINT('Ctrl Pts',(5.04970898462424,-0.262122881932824,
4.56119609516527));
#31325=CARTESIAN_POINT('Ctrl Pts',(5.07356690265566,-0.498968457612796,
4.36698765751594));
#31326=CARTESIAN_POINT('Ctrl Pts',(5.09742482068708,-0.613802653778546,
4.08304074106085));
#31327=CARTESIAN_POINT('Ctrl Pts',(5.12128273871849,-0.578545381446849,
3.77878810143205));
#31328=CARTESIAN_POINT('Ctrl Pts',(5.14514065674992,-0.40181800409162,3.52862779669421));
#31329=CARTESIAN_POINT('Ctrl Pts',(5.16899857478133,-0.126835179433317,
3.39373083558568));
#31330=CARTESIAN_POINT('Ctrl Pts',(5.19285649281276,0.179162301517353,3.4070831996169));
#31331=CARTESIAN_POINT('Ctrl Pts',(5.21671441084417,0.441349719463922,3.56541987207117));
#31332=CARTESIAN_POINT('Ctrl Pts',(5.24057232887559,0.595615108876583,3.83002322352904));
#31333=CARTESIAN_POINT('Ctrl Pts',(5.26443024690701,0.604236379939102,4.13619052690848));
#31334=CARTESIAN_POINT('Ctrl Pts',(5.28828816493843,0.465105397037983,4.40905553670335));
#31335=CARTESIAN_POINT('Ctrl Pts',(5.31214608296985,0.21224347534444,4.58189532532512));
#31336=CARTESIAN_POINT('Ctrl Pts',(5.33600400100126,-0.0925177574670201,
4.61244585639451));
#31337=CARTESIAN_POINT('Ctrl Pts',(5.35986191903269,-0.37465587844466,4.49323669288525));
#31338=CARTESIAN_POINT('Ctrl Pts',(5.3837198370641,-0.565180431721392,4.25341772246777));
#31339=CARTESIAN_POINT('Ctrl Pts',(5.40757775509553,-0.617502974236318,
3.95163121594683));
#31340=CARTESIAN_POINT('Ctrl Pts',(5.43143567312694,-0.518829219107294,
3.66167219466597));
#31341=CARTESIAN_POINT('Ctrl Pts',(5.45529359115837,-0.293287587282116,
3.45444353765392));
#31342=CARTESIAN_POINT('Ctrl Pts',(5.47915150918978,0.00397084862654925,
3.38061829634467));
#31343=CARTESIAN_POINT('Ctrl Pts',(5.50300942722121,0.300258303883157,3.45824875319892));
#31344=CARTESIAN_POINT('Ctrl Pts',(5.52686734525262,0.523124424966688,3.66835214690199));
#31345=CARTESIAN_POINT('Ctrl Pts',(5.55072526328404,0.618072374525773,3.95955247459688));
#31346=CARTESIAN_POINT('Ctrl Pts',(5.57458318131546,0.561884792553919,4.26064332401524));
#31347=CARTESIAN_POINT('Ctrl Pts',(5.59844109934688,0.368301073379394,4.49799978094171));
#31348=CARTESIAN_POINT('Ctrl Pts',(5.62229901737829,0.0846577094226282,
4.61358172616469));
#31349=CARTESIAN_POINT('Ctrl Pts',(5.64615693540972,-0.219686770477705,
4.57912622575047));
#31350=CARTESIAN_POINT('Ctrl Pts',(5.67001485344113,-0.470311850924231,
4.40305858798173));
#31351=CARTESIAN_POINT('Ctrl Pts',(5.69387277147256,-0.605932872639677,
4.12843214650112));
#31352=CARTESIAN_POINT('Ctrl Pts',(5.71773068950397,-0.593386801983745,
3.82240054650545));
#31353=CARTESIAN_POINT('Ctrl Pts',(5.74158860753539,-0.435741494202748,
3.55979685111874));
#31354=CARTESIAN_POINT('Ctrl Pts',(5.76544652556682,-0.171545522688555,
3.40483481554927));
#31355=CARTESIAN_POINT('Ctrl Pts',(5.78930444359822,0.134598003740687,3.39540688139736));
#31356=CARTESIAN_POINT('Ctrl Pts',(5.81316236162965,0.407828648458881,3.53381843004554));
#31357=CARTESIAN_POINT('Ctrl Pts',(5.83702027966106,0.58133408605803,3.78622407765735));
#31358=CARTESIAN_POINT('Ctrl Pts',(5.86087819769249,0.612687492198482,4.09090374899912));
#31359=CARTESIAN_POINT('Ctrl Pts',(5.8847361157239,0.494222140250734,4.3733550009975));
#31360=CARTESIAN_POINT('Ctrl Pts',(5.90859403375532,0.254905969192102,4.56451074097759));
#31361=CARTESIAN_POINT('Ctrl Pts',(5.93245195178675,-0.0467415727364197,
4.61762831145024));
#31362=CARTESIAN_POINT('Ctrl Pts',(5.95630986981815,-0.336959681931401,
4.51971877801409));
#31363=CARTESIAN_POINT('Ctrl Pts',(5.98016778784959,-0.544781677596122,
4.29472414464893));
#31364=CARTESIAN_POINT('Ctrl Pts',(6.00402570588099,-0.61939026621187,3.99766086682344));
#31365=CARTESIAN_POINT('Ctrl Pts',(6.02788362391242,-0.542540019317823,
3.70117063377655));
#31366=CARTESIAN_POINT('Ctrl Pts',(6.05174154194384,-0.333025929677459,
3.47775031355921));
#31367=CARTESIAN_POINT('Ctrl Pts',(6.07559945997526,-0.042074208138152,
3.38203805739984));
#31368=CARTESIAN_POINT('Ctrl Pts',(6.09945737800668,0.259158778028439,3.43742717299816));
#31369=CARTESIAN_POINT('Ctrl Pts',(6.12331529603809,0.497033648893269,3.63039418124561));
#31370=CARTESIAN_POINT('Ctrl Pts',(6.14717321406952,0.613345206175343,3.91371436613889));
#31371=CARTESIAN_POINT('Ctrl Pts',(6.17103113210093,0.579724447951105,4.21818191418763));
#31372=CARTESIAN_POINT('Ctrl Pts',(6.19488905013236,0.40425597056565,4.46920707734689));
#31373=CARTESIAN_POINT('Ctrl Pts',(6.21874696816377,0.13010450107023,4.60567007851858));
#31374=CARTESIAN_POINT('Ctrl Pts',(6.24260488619519,-0.176179318911185,
4.59370602015056));
#31375=CARTESIAN_POINT('Ctrl Pts',(6.26646280422661,-0.438782409775579,
4.43717629804221));
#31376=CARTESIAN_POINT('Ctrl Pts',(6.29032072225803,-0.595217424383659,
4.17259489198797));
#31377=CARTESIAN_POINT('Ctrl Pts',(6.31417864028945,-0.604035436411749,
3.86794272465182));
#31378=CARTESIAN_POINT('Ctrl Pts',(6.34598919766468,-0.423477061217623,
3.4998212904071));
#31379=CARTESIAN_POINT('Ctrl Pts',(6.3857523943837,0.100470573235224,3.30464850830547));
#31380=CARTESIAN_POINT('Ctrl Pts',(6.43346823044655,0.640013163212275,3.70919899990029));
#31381=CARTESIAN_POINT('Ctrl Pts',(6.48118406650937,0.590335835129396,4.3806576914582));
#31382=CARTESIAN_POINT('Ctrl Pts',(6.52889990257223,-0.000686065451295705,
4.70262946694599));
#31383=CARTESIAN_POINT('Ctrl Pts',(6.57661573863505,-0.591483599613884,
4.37932465573422));
#31384=CARTESIAN_POINT('Ctrl Pts',(6.6243315746979,-0.638898060441451,3.70770201230499));
#31385=CARTESIAN_POINT('Ctrl Pts',(6.67204741076074,-0.0997162142428727,
3.30448953810453));
#31386=CARTESIAN_POINT('Ctrl Pts',(6.71976324682356,0.531096731682035,3.53998115137447));
#31387=CARTESIAN_POINT('Ctrl Pts',(6.76747908288643,0.674163513320998,4.19791190586338));
#31388=CARTESIAN_POINT('Ctrl Pts',(6.81519491894923,0.19815244237474,4.67409883091767));
#31389=CARTESIAN_POINT('Ctrl Pts',(6.86291075501209,-0.459834002450772,
4.53124951681343));
#31390=CARTESIAN_POINT('Ctrl Pts',(6.91062659107492,-0.695543074258338,
3.90054607923755));
#31391=CARTESIAN_POINT('Ctrl Pts',(6.95834242713776,-0.292526745343327,
3.36117245204842));
#31392=CARTESIAN_POINT('Ctrl Pts',(7.00605826320061,0.379122722467859,3.40844412700009));
#31393=CARTESIAN_POINT('Ctrl Pts',(7.05377409926343,0.702617257610868,3.99895059076549));
#31394=CARTESIAN_POINT('Ctrl Pts',(7.10148993532628,0.380887926283931,4.59042078110798));
#31395=CARTESIAN_POINT('Ctrl Pts',(7.14920577138911,-0.290616845661789,
4.63969846327979));
#31396=CARTESIAN_POINT('Ctrl Pts',(7.19692160745196,-0.695243592084394,
4.10153121423426));
#31397=CARTESIAN_POINT('Ctrl Pts',(7.24463744351478,-0.461417505508394,
3.47012628326466));
#31398=CARTESIAN_POINT('Ctrl Pts',(7.29235327957764,0.196135405489393,3.32531254251214));
#31399=CARTESIAN_POINT('Ctrl Pts',(7.34006911564046,0.673574140181709,3.80007467379138));
#31400=CARTESIAN_POINT('Ctrl Pts',(7.38778495170331,0.532459385890787,4.45843130921146));
#31401=CARTESIAN_POINT('Ctrl Pts',(7.43550078776614,-0.0976210197556089,
4.69580341906706));
#31402=CARTESIAN_POINT('Ctrl Pts',(7.48321662382899,-0.638054538563543,
4.29420854311633));
#31403=CARTESIAN_POINT('Ctrl Pts',(7.53093245989182,-0.592552758097988,
3.62243743491725));
#31404=CARTESIAN_POINT('Ctrl Pts',(7.57864829595465,-0.00290066162856385,
3.29738783984629));
#31405=CARTESIAN_POINT('Ctrl Pts',(7.6263641320175,0.589415156704478,3.61755780248734));
#31406=CARTESIAN_POINT('Ctrl Pts',(7.67407996808033,0.64046196749915,4.28893031975233));
#31407=CARTESIAN_POINT('Ctrl Pts',(7.72179580414318,0.103362698669259,4.69497367861456));
#31408=CARTESIAN_POINT('Ctrl Pts',(7.769511640206,-0.528656126737314,4.46281201486565));
#31409=CARTESIAN_POINT('Ctrl Pts',(7.81722747626886,-0.675201896567852,
3.80564295658466));
#31410=CARTESIAN_POINT('Ctrl Pts',(7.86494331233168,-0.201699375449268,
3.32695496184095));
#31411=CARTESIAN_POINT('Ctrl Pts',(7.91265914839452,0.457026785680635,3.46633458176699));
#31412=CARTESIAN_POINT('Ctrl Pts',(7.96037498445737,0.696058217263005,4.09578736675475));
#31413=CARTESIAN_POINT('Ctrl Pts',(8.0080908205202,0.295888677698302,4.63727713897333));
#31414=CARTESIAN_POINT('Ctrl Pts',(8.05580665658303,-0.375999987428149,
4.59354550870361));
#31415=CARTESIAN_POINT('Ctrl Pts',(8.10352249264589,-0.702602078596463,
4.00475190491975));
#31416=CARTESIAN_POINT('Ctrl Pts',(8.1512383287087,-0.383993870066737,3.41159455373064));
#31417=CARTESIAN_POINT('Ctrl Pts',(8.19895416477156,0.287241817850264,3.35877897763223));
#31418=CARTESIAN_POINT('Ctrl Pts',(8.24667000083438,0.694698924651979,3.89480653282778));
#31419=CARTESIAN_POINT('Ctrl Pts',(8.29438583689724,0.464203319628796,4.52743486753713));
#31420=CARTESIAN_POINT('Ctrl Pts',(8.34210167296006,-0.192577336495663,
4.67571164775853));
#31421=CARTESIAN_POINT('Ctrl Pts',(8.3898175090229,-0.672511261332963,4.20347202468314));
#31422=CARTESIAN_POINT('Ctrl Pts',(8.43753334508575,-0.534867746972347,
3.54438091052171));
#31423=CARTESIAN_POINT('Ctrl Pts',(8.48524918114857,0.0939530494311211,
3.303691816829));
#31424=CARTESIAN_POINT('Ctrl Pts',(8.53296501721143,0.636495314888509,3.70243324182078));
#31425=CARTESIAN_POINT('Ctrl Pts',(8.58068085327425,0.594534138944492,4.37443479950165));
#31426=CARTESIAN_POINT('Ctrl Pts',(8.6283966893371,0.00660311512414562,
4.7025871193802));
#31427=CARTESIAN_POINT('Ctrl Pts',(8.67611252539993,-0.58739165091669,4.3855428768395));
#31428=CARTESIAN_POINT('Ctrl Pts',(8.72382836146277,-0.64197562573843,3.71444867815739));
#31429=CARTESIAN_POINT('Ctrl Pts',(8.77154419752561,-0.107023505379864,
3.30558065209521));
#31430=CARTESIAN_POINT('Ctrl Pts',(8.81926003358845,0.526209946737336,3.53440859822909));
#31431=CARTESIAN_POINT('Ctrl Pts',(8.86697586965128,0.676216707984864,4.19079629265377));
#31432=CARTESIAN_POINT('Ctrl Pts',(8.91469170571413,0.20524326135842,4.67197281575615));
#31433=CARTESIAN_POINT('Ctrl Pts',(8.96240754177695,-0.45420823024697,4.53606636251889));
#31434=CARTESIAN_POINT('Ctrl Pts',(9.0101233778398,-0.69655331512461,3.90788192013928));
#31435=CARTESIAN_POINT('Ctrl Pts',(9.05783921390263,-0.299242772872918,
3.36429092791464));
#31436=CARTESIAN_POINT('Ctrl Pts',(9.10555504996548,0.37286701214988,3.40448135822736));
#31437=CARTESIAN_POINT('Ctrl Pts',(9.15327088602831,0.702567282619003,3.99154572051203));
#31438=CARTESIAN_POINT('Ctrl Pts',(9.20098672209116,0.387089207071907,4.58637377773631));
#31439=CARTESIAN_POINT('Ctrl Pts',(9.24870255815397,-0.28385884346236,4.64272577234503));
#31440=CARTESIAN_POINT('Ctrl Pts',(9.29641839421684,-0.694134950315416,
4.10885280060212));
#31441=CARTESIAN_POINT('Ctrl Pts',(9.34413423027966,-0.46697625165475,3.47501862715065));
#31442=CARTESIAN_POINT('Ctrl Pts',(9.39185006634251,0.189013924253689,3.32328292626348));
#31443=CARTESIAN_POINT('Ctrl Pts',(9.43956590240535,0.671429705166911,3.79298692681914));
#31444=CARTESIAN_POINT('Ctrl Pts',(9.48728173846818,0.537261256551386,4.45279421778236));
#31445=CARTESIAN_POINT('Ctrl Pts',(9.53499757453101,-0.090282470782305,
4.69679361142145));
#31446=CARTESIAN_POINT('Ctrl Pts',(9.58271341059386,-0.634918416022234,
4.30091671014441));
#31447=CARTESIAN_POINT('Ctrl Pts',(9.63042924665669,-0.596499010353368,
3.62870336374299));
#31448=CARTESIAN_POINT('Ctrl Pts',(9.67814508271953,-0.0103053851599677,
3.29745743154951));
#31449=CARTESIAN_POINT('Ctrl Pts',(9.72586091878236,0.585351833794561,3.61136714997101));
#31450=CARTESIAN_POINT('Ctrl Pts',(9.77357675484522,0.643471456979869,4.28216439445919));
#31451=CARTESIAN_POINT('Ctrl Pts',(9.82129259090803,0.110681340139534,4.69384573385819));
#31452=CARTESIAN_POINT('Ctrl Pts',(9.8690084269709,-0.523749154402255,4.46835785966634));
#31453=CARTESIAN_POINT('Ctrl Pts',(9.91672426303372,-0.677212741539845,
3.81276975633088));
#31454=CARTESIAN_POINT('Ctrl Pts',(9.96444009909655,-0.208781447863971,
3.32911806666439));
#31455=CARTESIAN_POINT('Ctrl Pts',(10.0121559351594,0.451377061900895,3.4615475792254));
#31456=CARTESIAN_POINT('Ctrl Pts',(10.0598717712222,0.697029070393332,4.08844623493918));
#31457=CARTESIAN_POINT('Ctrl Pts',(10.1075876072851,0.302588558372737,4.63412335218805));
#31458=CARTESIAN_POINT('Ctrl Pts',(10.1553034433479,-0.369723682724971,
4.5974752378807));
#31459=CARTESIAN_POINT('Ctrl Pts',(10.2030192794108,-0.702512977046242,
4.01215641928927));
#31460=CARTESIAN_POINT('Ctrl Pts',(10.2507351154736,-0.390173794994359,
3.41567417381395));
#31461=CARTESIAN_POINT('Ctrl Pts',(10.2984509515364,0.280467986596366,3.3557873255338));
#31462=CARTESIAN_POINT('Ctrl Pts',(10.3461667875993,0.693551700540965,3.8874908887021));
#31463=CARTESIAN_POINT('Ctrl Pts',(10.3938826236621,0.469736216214169,4.52251329995044));
#31464=CARTESIAN_POINT('Ctrl Pts',(10.441598459725,-0.185445263282835,4.67770370795377));
#31465=CARTESIAN_POINT('Ctrl Pts',(10.4893142957878,-0.670329504065059,
4.21054837313121));
#31466=CARTESIAN_POINT('Ctrl Pts',(10.5370301318506,-0.539639846919137,
3.55004322755915));
#31467=CARTESIAN_POINT('Ctrl Pts',(10.5847459679134,0.0866093850789692,
3.30274030959437));
#31468=CARTESIAN_POINT('Ctrl Pts',(10.6324618039763,0.633323886102378,3.69574169404847));
#31469=CARTESIAN_POINT('Ctrl Pts',(10.6801776400391,0.598447317577389,4.36814816247366));
#31470=CARTESIAN_POINT('Ctrl Pts',(10.727893476102,0.0140073690254923,4.70247850861168));
#31471=CARTESIAN_POINT('Ctrl Pts',(10.7756093121648,-0.583295762033595,
4.39171203127037));
#31472=CARTESIAN_POINT('Ctrl Pts',(10.8233251482277,-0.644949419658282,
3.72123036834915));
#31473=CARTESIAN_POINT('Ctrl Pts',(10.8710409842905,-0.114336101388361,
3.30674714759503));
#31474=CARTESIAN_POINT('Ctrl Pts',(10.9187568203533,0.521273818073547,3.52888868827067));
#31475=CARTESIAN_POINT('Ctrl Pts',(10.9664726564162,0.678189969569843,4.18365899548663));
#31476=CARTESIAN_POINT('Ctrl Pts',(11.014188492479,0.212313836716152,4.66977242119035));
#31477=CARTESIAN_POINT('Ctrl Pts',(11.0619043285418,-0.44853335926228,4.54082352674158));
#31478=CARTESIAN_POINT('Ctrl Pts',(11.1096201646047,-0.697485469857315,
3.91522806604643));
#31479=CARTESIAN_POINT('Ctrl Pts',(11.1573360006675,-0.305925941288932,
3.36747997668469));
#31480=CARTESIAN_POINT('Ctrl Pts',(11.2050518367303,0.36657008644075,3.40058475730499));
#31481=CARTESIAN_POINT('Ctrl Pts',(11.2527676727932,0.702439163386103,3.98414177848112));
#31482=CARTESIAN_POINT('Ctrl Pts',(11.300483508856,0.393247548178179,4.58226164848818));
#31483=CARTESIAN_POINT('Ctrl Pts',(11.3481993449189,-0.277069341413063,
4.64568168744144));
#31484=CARTESIAN_POINT('Ctrl Pts',(11.3959151809817,-0.692949191524882,
4.11616229772746));
#31485=CARTESIAN_POINT('Ctrl Pts',(11.4436310170446,-0.47248313666557,3.47996928262364));
#31486=CARTESIAN_POINT('Ctrl Pts',(11.4913468531074,0.181871452681271,3.32132847698764));
#31487=CARTESIAN_POINT('Ctrl Pts',(11.5390626891702,0.669210688578896,3.78592217363756));
#31488=CARTESIAN_POINT('Ctrl Pts',(11.586778525233,0.54200345202451,4.44710683224685));
#31489=CARTESIAN_POINT('Ctrl Pts',(11.6344943612959,-0.082933894319074,
4.69770640718098));
#31490=CARTESIAN_POINT('Ctrl Pts',(11.6822101973587,-0.631711769407458,
4.30759145280778));
#31491=CARTESIAN_POINT('Ctrl Pts',(11.7299260334216,-0.600379006513997,
3.63501053441836));
#31492=CARTESIAN_POINT('Ctrl Pts',(11.7776418694844,-0.0177089639202829,
3.29760505835735));
#31493=CARTESIAN_POINT('Ctrl Pts',(11.8253577055473,0.581223492728864,3.60521966494218));
#31494=CARTESIAN_POINT('Ctrl Pts',(11.8730735416101,0.646409472732109,4.27536712768685));
#31495=CARTESIAN_POINT('Ctrl Pts',(11.9207893776729,0.11798768763725,4.69264072000881));
#31496=CARTESIAN_POINT('Ctrl Pts',(11.9685052137358,-0.518784006488825,
4.4738516814993));
#31497=CARTESIAN_POINT('Ctrl Pts',(12.0162210497986,-0.679148364938221,
3.81991735272367));
#31498=CARTESIAN_POINT('Ctrl Pts',(12.0639368858614,-0.215840329824027,
3.33135568986959));
#31499=CARTESIAN_POINT('Ctrl Pts',(12.1116527219243,0.445677201297934,3.45682038542343));
#31500=CARTESIAN_POINT('Ctrl Pts',(12.1593685579871,0.697922500842799,4.08109527893561));
#31501=CARTESIAN_POINT('Ctrl Pts',(12.2070843940499,0.309254828945687,4.63089912998995));
#31502=CARTESIAN_POINT('Ctrl Pts',(12.2548002301128,-0.36340631086944,4.60133860234362));
#31503=CARTESIAN_POINT('Ctrl Pts',(12.3025160661756,-0.702345843688318,
4.0195595833814));
#31504=CARTESIAN_POINT('Ctrl Pts',(12.3502319022385,-0.396310381268302,
3.41981869803717));
#31505=CARTESIAN_POINT('Ctrl Pts',(12.3979477383013,0.273663002289436,3.35286722952223));
#31506=CARTESIAN_POINT('Ctrl Pts',(12.4456635743641,0.69232743999824,3.88018774155459));
#31507=CARTESIAN_POINT('Ctrl Pts',(12.493379410427,0.475216936729713,4.51753369406595));
#31508=CARTESIAN_POINT('Ctrl Pts',(12.5410952464898,-0.178292591690169,
4.67962049203707));
#31509=CARTESIAN_POINT('Ctrl Pts',(12.5888110825527,-0.66807328977682,4.21760133486514));
#31510=CARTESIAN_POINT('Ctrl Pts',(12.6365269186155,-0.544352006232531,
3.55575552365962));
#31511=CARTESIAN_POINT('Ctrl Pts',(12.6842427546784,0.0792561005673328,
3.3018662506574));
#31512=CARTESIAN_POINT('Ctrl Pts',(12.7319585907411,0.630082110704352,3.68908394184497));
#31513=CARTESIAN_POINT('Ctrl Pts',(12.779674426804,0.60229402352211,4.36182063329482));
#31514=CARTESIAN_POINT('Ctrl Pts',(12.8273902628668,0.0214100670547408,
4.70229186986395));
#31515=CARTESIAN_POINT('Ctrl Pts',(12.8751060989297,-0.579135083425219,
4.39783767618763));
#31516=CARTESIAN_POINT('Ctrl Pts',(12.9228219349925,-0.647851575657132,
3.7280430229487));
#31517=CARTESIAN_POINT('Ctrl Pts',(12.9705377710554,-0.121635997485283,
3.30799064633195));
#31518=CARTESIAN_POINT('Ctrl Pts',(13.0182536071182,0.516279788787698,3.52342110712114));
#31519=CARTESIAN_POINT('Ctrl Pts',(13.065969443181,0.68008790103128,4.17650129834983));
#31520=CARTESIAN_POINT('Ctrl Pts',(13.1136852792439,0.219360829260397,4.66749763148232));
#31521=CARTESIAN_POINT('Ctrl Pts',(13.1614011153067,-0.44280866732052,4.54552061885334));
#31522=CARTESIAN_POINT('Ctrl Pts',(13.2091169513696,-0.698340151213866,
3.92258362801769));
#31523=CARTESIAN_POINT('Ctrl Pts',(13.2568327874324,-0.31257512890311,3.37073928277739));
#31524=CARTESIAN_POINT('Ctrl Pts',(13.3045486234952,0.36023244386594,3.39675473658331));
#31525=CARTESIAN_POINT('Ctrl Pts',(13.3522644595581,0.702233020544282,3.97673959790624));
#31526=CARTESIAN_POINT('Ctrl Pts',(13.3999802956209,0.39936220921291,4.57808484437918));
#31527=CARTESIAN_POINT('Ctrl Pts',(13.4476961316837,-0.270249063816132,
4.64856588328003));
#31528=CARTESIAN_POINT('Ctrl Pts',(13.4954119677466,-0.691686463226468,
4.123458892096));
#31529=CARTESIAN_POINT('Ctrl Pts',(13.5431278038094,-0.47793754049168,3.48497770064095));
#31530=CARTESIAN_POINT('Ctrl Pts',(13.5908436398723,0.174708779690948,3.31944941132403));
#31531=CARTESIAN_POINT('Ctrl Pts',(13.6385594759351,0.666917339243262,3.77888119920505));
#31532=CARTESIAN_POINT('Ctrl Pts',(13.6862753119979,0.54668544432619,4.44136978420615));
#31533=CARTESIAN_POINT('Ctrl Pts',(13.7339911480608,-0.075576105952426,
4.69854170502367));
#31534=CARTESIAN_POINT('Ctrl Pts',(13.7817069841236,-0.62843495524706,4.31423202967224));
#31535=CARTESIAN_POINT('Ctrl Pts',(13.8294228201864,-0.604192315423611,
3.64135824639153));
#31536=CARTESIAN_POINT('Ctrl Pts',(13.8771386562493,-0.025110575652917,
3.29783070386218));
#31537=CARTESIAN_POINT('Ctrl Pts',(13.9248544923121,0.577030592115723,3.59911603023956));
#31538=CARTESIAN_POINT('Ctrl Pts',(13.972570328375,0.649275688387581,4.26853927444071));
#31539=CARTESIAN_POINT('Ctrl Pts',(14.0202861644378,0.125280929622514,4.69135877091509));
#31540=CARTESIAN_POINT('Ctrl Pts',(14.0680020005006,-0.513761234509794,
4.47929287013608));
#31541=CARTESIAN_POINT('Ctrl Pts',(14.1157178365635,-0.681008551759042,
3.82708495184235));
#31542=CARTESIAN_POINT('Ctrl Pts',(14.1634336726263,-0.222875237264486,
3.33366758291179));
#31543=CARTESIAN_POINT('Ctrl Pts',(14.2111495086891,0.439927836986373,3.45215352543546));
#31544=CARTESIAN_POINT('Ctrl Pts',(14.258865344752,0.698738409372782,4.07373531525328));
#31545=CARTESIAN_POINT('Ctrl Pts',(14.3065811808148,0.315886748959774,4.62760483051036));
#31546=CARTESIAN_POINT('Ctrl Pts',(14.3542970168777,-0.357048573565392,
4.60513517296818));
#31547=CARTESIAN_POINT('Ctrl Pts',(14.4020128529405,-0.702100697086982,
4.02696057488784));
#31548=CARTESIAN_POINT('Ctrl Pts',(14.4497286890033,-0.402402947265751,
3.42402766604624));
#31549=CARTESIAN_POINT('Ctrl Pts',(14.4974445250662,0.266827620794843,3.35001901394789));
#31550=CARTESIAN_POINT('Ctrl Pts',(14.545160361129,0.691026279008849,3.87289790258421));
#31551=CARTESIAN_POINT('Ctrl Pts',(14.5928761971919,0.480644872403009,4.51249660299459));
#31552=CARTESIAN_POINT('Ctrl Pts',(14.6405920332547,-0.171120116202498,
4.6814617871012));
#31553=CARTESIAN_POINT('Ctrl Pts',(14.6883078693176,-0.665742869077823,
4.22463012647536));
#31554=CARTESIAN_POINT('Ctrl Pts',(14.7360237053803,-0.549003701508229,
3.56151716432844));
#31555=CARTESIAN_POINT('Ctrl Pts',(14.7837395414432,0.0718940126641393,
3.30106973710437));
#31556=CARTESIAN_POINT('Ctrl Pts',(14.831455377506,0.626770348775451,3.68246072472179));
#31557=CARTESIAN_POINT('Ctrl Pts',(14.8791712135689,0.606073829504824,4.35545291479698));
#31558=CARTESIAN_POINT('Ctrl Pts',(14.9268870496317,0.0288103869553486,
4.70202722386799));
#31559=CARTESIAN_POINT('Ctrl Pts',(14.9746028856946,-0.574910077240004,
4.4039191311837));
#31560=CARTESIAN_POINT('Ctrl Pts',(15.0223187217574,-0.650681771377263,
3.73488588523872));
#31561=CARTESIAN_POINT('Ctrl Pts',(15.0700345578202,-0.128922382832804,
3.30931101018402));
#31562=CARTESIAN_POINT('Ctrl Pts',(15.1177503938831,0.511228413592865,3.51800646209349));
#31563=CARTESIAN_POINT('Ctrl Pts',(15.1654662299459,0.681910291555949,4.16932399628639));
#31564=CARTESIAN_POINT('Ctrl Pts',(15.2131820660088,0.226383456244684,4.6651486993049));
#31565=CARTESIAN_POINT('Ctrl Pts',(15.2608979020716,-0.437034790293287,
4.55015711712348));
#31566=CARTESIAN_POINT('Ctrl Pts',(15.3086137381344,-0.699117264260319,
3.92994778903219));
#31567=CARTESIAN_POINT('Ctrl Pts',(15.3563295741972,-0.319189597155267,
3.37406848416447));
#31568=CARTESIAN_POINT('Ctrl Pts',(15.4040454102601,0.353854788380711,3.39299172148285));
#31569=CARTESIAN_POINT('Ctrl Pts',(15.4517612463229,0.70194887699091,3.96934000098645));
#31570=CARTESIAN_POINT('Ctrl Pts',(15.4994770823858,0.40543251098856,4.57384382934891));
#31571=CARTESIAN_POINT('Ctrl Pts',(15.5471929184486,-0.263398768235635,
4.65137803949801));
#31572=CARTESIAN_POINT('Ctrl Pts',(15.5949087545115,-0.690346905678043,
4.13074177323664));
#31573=CARTESIAN_POINT('Ctrl Pts',(15.6426245905743,-0.483338857283784,
3.4900433248913));
#31574=CARTESIAN_POINT('Ctrl Pts',(15.6903404266371,0.167526700878456,3.31764593799033));
#31575=CARTESIAN_POINT('Ctrl Pts',(15.7380562627,0.664549911894371,3.77186478559966));
#31576=CARTESIAN_POINT('Ctrl Pts',(15.7857720987628,0.551306713402943,4.43558371090429));
#31577=CARTESIAN_POINT('Ctrl Pts',(15.8334879348256,-0.0682099229505586,
4.69929941216862));
#31578=CARTESIAN_POINT('Ctrl Pts',(15.8812037708885,-0.625088337514006,
4.32083770313399));
#31579=CARTESIAN_POINT('Ctrl Pts',(15.9289196069513,-0.607938513517956,
3.64774579458877));
#31580=CARTESIAN_POINT('Ctrl Pts',(15.9766354430142,-0.0325093982219456,
3.29813434300035));
#31581=CARTESIAN_POINT('Ctrl Pts',(16.024351279077,0.572773597682653,3.59305692382598));
#31582=CARTESIAN_POINT('Ctrl Pts',(16.0720671151399,0.652069785580651,4.2616815931263));
#31583=CARTESIAN_POINT('Ctrl Pts',(16.1197829512026,0.132560255996602,4.69000002896988));
#31584=CARTESIAN_POINT('Ctrl Pts',(16.1674987872655,-0.508681396370837,
4.48468082119526));
#31585=CARTESIAN_POINT('Ctrl Pts',(16.2152146233283,-0.682793095381579,
3.83427175754402));
#31586=CARTESIAN_POINT('Ctrl Pts',(16.2629304593912,-0.229885388781225,
3.33605348899688));
#31587=CARTESIAN_POINT('Ctrl Pts',(16.310646295454,0.434129607578297,3.44754751763412));
#31588=CARTESIAN_POINT('Ctrl Pts',(16.3583621315168,0.699476705356048,4.06636716140204));
#31589=CARTESIAN_POINT('Ctrl Pts',(16.4060779675797,0.322483581772784,4.62424081966442));
#31590=CARTESIAN_POINT('Ctrl Pts',(16.4537938036425,-0.350651177000141,
4.60886452804932));
#31591=CARTESIAN_POINT('Ctrl Pts',(16.5015096397054,-0.701777564471952,
4.03435857174156));
#31592=CARTESIAN_POINT('Ctrl Pts',(16.5492254757682,-0.408450816253369,
3.42830061032894));
#31593=CARTESIAN_POINT('Ctrl Pts',(16.596941311831,0.259962601354342,3.34724299517707));
#31594=CARTESIAN_POINT('Ctrl Pts',(16.6446571478939,0.689648362099571,3.86562218151166));
#31595=CARTESIAN_POINT('Ctrl Pts',(16.6923729839567,0.486019420324727,4.50740258623259));
#31596=CARTESIAN_POINT('Ctrl Pts',(16.7400888200196,-0.163928633504336,
4.6832273886238));
#31597=CARTESIAN_POINT('Ctrl Pts',(16.7878046560824,-0.663338500820136,
4.23163396723712));
#31598=CARTESIAN_POINT('Ctrl Pts',(16.8355204921452,-0.553594416058007,
3.56732750958986));
#31599=CARTESIAN_POINT('Ctrl Pts',(16.8832363282081,0.064523939115192,3.30035085740826));
#31600=CARTESIAN_POINT('Ctrl Pts',(16.9309521642709,0.623388968170475,3.67587277835446));
#31601=CARTESIAN_POINT('Ctrl Pts',(16.9786680003338,0.609786315682611,4.34904571427615));
#31602=CARTESIAN_POINT('Ctrl Pts',(17.0263838363966,0.0362075067348799,
4.70168460001938));
#31603=CARTESIAN_POINT('Ctrl Pts',(17.0740996724594,-0.570621212771584,
4.40995572075944));
#31604=CARTESIAN_POINT('Ctrl Pts',(17.1218155085223,-0.653439692453966,
3.74175819514654));
#31605=CARTESIAN_POINT('Ctrl Pts',(17.1695313445851,-0.136194448093839,
3.31070809249149));
#31606=CARTESIAN_POINT('Ctrl Pts',(17.2172471806479,0.50612025357182,3.51264535462077));
#31607=CARTESIAN_POINT('Ctrl Pts',(17.2649630167108,0.683656938721366,4.16212788651693));
#31608=CARTESIAN_POINT('Ctrl Pts',(17.3126788527736,0.233380937628925,4.66272588556639));
#31609=CARTESIAN_POINT('Ctrl Pts',(17.3603946888365,-0.431212369515449,
4.55473250655174));
#31610=CARTESIAN_POINT('Ctrl Pts',(17.4081105248993,-0.699816722678643,
3.93731973111387));
#31611=CARTESIAN_POINT('Ctrl Pts',(17.4558263609621,-0.325768611341644,
3.37746721105403));
#31612=CARTESIAN_POINT('Ctrl Pts',(17.503542197025,0.347437828384778,3.38929612998149));
#31613=CARTESIAN_POINT('Ctrl Pts',(17.5512580330878,0.701586764287296,3.96194380963385));
#31614=CARTESIAN_POINT('Ctrl Pts',(17.5989738691507,0.411457779244836,4.56953907446917));
#31615=CARTESIAN_POINT('Ctrl Pts',(17.6466897052135,-0.256519215569882,
4.65411784373439));
#31616=CARTESIAN_POINT('Ctrl Pts',(17.6944055412764,-0.688930667671302,
4.13801013220155));
#31617=CARTESIAN_POINT('Ctrl Pts',(17.7421213773391,-0.488686487089258,
3.49516559270919));
#31618=CARTESIAN_POINT('Ctrl Pts',(17.789837213402,0.160326013994967,3.3159182573078));
#31619=CARTESIAN_POINT('Ctrl Pts',(17.8375530494648,0.662108669494809,3.76487371217125));
#31620=CARTESIAN_POINT('Ctrl Pts',(17.8852688855277,0.555866745946156,4.42974925503083));
#31621=CARTESIAN_POINT('Ctrl Pts',(17.9329847215905,-0.060836163514142,
4.69997944445332));
#31622=CARTESIAN_POINT('Ctrl Pts',(17.9807005576534,-0.621672287934692,
4.32740773946617));
#31623=CARTESIAN_POINT('Ctrl Pts',(18.0284163937162,-0.611617184687133,
3.65417246951162));
#31624=CARTESIAN_POINT('Ctrl Pts',(18.0761322297791,-0.0399046098013318,
3.29851594204507));
#31625=CARTESIAN_POINT('Ctrl Pts',(18.1238480658419,0.568452982276385,3.58704301871817));
#31626=CARTESIAN_POINT('Ctrl Pts',(18.1715639019047,0.65479145395626,4.25479484546229));
#31627=CARTESIAN_POINT('Ctrl Pts',(18.2192797379675,0.139824858206545,4.68856464509573));
#31628=CARTESIAN_POINT('Ctrl Pts',(18.2669955740304,-0.503545056316242,
4.49001493620888));
#31629=CARTESIAN_POINT('Ctrl Pts',(18.3147114100932,-0.684501797587214,
3.84147697155243));
#31630=CARTESIAN_POINT('Ctrl Pts',(18.3624272461561,-0.236870005719869,
3.33851314310973));
#31631=CARTESIAN_POINT('Ctrl Pts',(18.4101430822189,0.42828315711354,3.44300287363294));
#31632=CARTESIAN_POINT('Ctrl Pts',(18.4578589182817,0.70013730678616,4.05899163580144));
#31633=CARTESIAN_POINT('Ctrl Pts',(18.5055747543446,0.32904459463985,4.62080747111051));
#31634=CARTESIAN_POINT('Ctrl Pts',(18.5532905904074,-0.34421483176614,4.61252625334797));
#31635=CARTESIAN_POINT('Ctrl Pts',(18.6010064264702,-0.701376481735239,
4.0417527522082));
#31636=CARTESIAN_POINT('Ctrl Pts',(18.6487222625331,-0.414453316462639,
3.43263705626685));
#31637=CARTESIAN_POINT('Ctrl Pts',(18.6964380985959,0.253068706501803,3.34453948155689));
#31638=CARTESIAN_POINT('Ctrl Pts',(18.7441539346588,0.68819384232267,3.85836138648927));
#31639=CARTESIAN_POINT('Ctrl Pts',(18.7918697707216,0.491339983515996,4.50225220959958));
#31640=CARTESIAN_POINT('Ctrl Pts',(18.8395856067844,-0.156718942392259,
4.68491710048942));
#31641=CARTESIAN_POINT('Ctrl Pts',(18.8873014428473,-0.660860452068119,
4.23861207919858));
#31642=CARTESIAN_POINT('Ctrl Pts',(18.9350172789101,-0.558123639969822,
3.57318591405529));
#31643=CARTESIAN_POINT('Ctrl Pts',(18.9827331149729,0.0571466985584877,
3.29970969142451));
#31644=CARTESIAN_POINT('Ctrl Pts',(19.0304489510358,0.619938344467307,3.66932083449001));
#31645=CARTESIAN_POINT('Ctrl Pts',(19.0781647870986,0.613431069708698,4.3425997434341));
#31646=CARTESIAN_POINT('Ctrl Pts',(19.1258806231615,0.0436006047213211,
4.70126403633668));
#31647=CARTESIAN_POINT('Ctrl Pts',(19.1735964592243,-0.566268966340429,
4.41594677447179));
#31648=CARTESIAN_POINT('Ctrl Pts',(19.2213122952871,-0.656125032675529,
3.74865918919138));
#31649=CARTESIAN_POINT('Ctrl Pts',(19.26902813135,-0.143451385285705,3.31218173833215));
#31650=CARTESIAN_POINT('Ctrl Pts',(19.3167439674128,0.500955875668841,3.50733837970023));
#31651=CARTESIAN_POINT('Ctrl Pts',(19.3644598034757,0.68532764936022,4.15491376927485));
#31652=CARTESIAN_POINT('Ctrl Pts',(19.4121756395385,0.240352494576274,4.66022945763735));
#31653=CARTESIAN_POINT('Ctrl Pts',(19.4598914756013,-0.425342048711971,
4.55924628221868));
#31654=CARTESIAN_POINT('Ctrl Pts',(19.5076073116642,-0.700438454444525,
3.94469862920436));
#31655=CARTESIAN_POINT('Ctrl Pts',(19.555323147727,-0.332311429993836,3.3809350976725));
#31656=CARTESIAN_POINT('Ctrl Pts',(19.6030389837899,0.340982256434611,3.38566835039883));
#31657=CARTESIAN_POINT('Ctrl Pts',(19.6507548198527,0.701146760813864,3.95455188724214));
#31658=CARTESIAN_POINT('Ctrl Pts',(19.6984706559155,0.417437272672218,4.56517097885182));
#31659=CARTESIAN_POINT('Ctrl Pts',(19.7461864919784,-0.249611033919464,
4.6567851409082));
#31660=CARTESIAN_POINT('Ctrl Pts',(19.7939023280412,-0.687438163400574,
4.14526287985386));
#31661=CARTESIAN_POINT('Ctrl Pts',(19.841618164104,-0.493979350866992,3.5003444672369));
#31662=CARTESIAN_POINT('Ctrl Pts',(19.8893340001669,0.153106602982307,3.31426555646693));
#31663=CARTESIAN_POINT('Ctrl Pts',(19.9370498362297,0.659595612567133,3.75791065255607));
#31664=CARTESIAN_POINT('Ctrl Pts',(19.9847656722925,0.560361770063263,4.42386348253578));
#31665=CARTESIAN_POINT('Ctrl Pts',(20.0324815083554,-0.0534494809679074,
4.70058849011268));
#31666=CARTESIAN_POINT('Ctrl Pts',(20.0801973444182,-0.618198828117398,
4.33392863744107));
#31667=CARTESIAN_POINT('Ctrl Pts',(20.1279131804811,-0.615205937201001,
3.66066167313574));
#31668=CARTESIAN_POINT('Ctrl Pts',(20.1756290165439,-0.0473369003220797,
3.29892991724937));
#31669=CARTESIAN_POINT('Ctrl Pts',(20.2233448526068,0.564147630203746,3.58116102158214));
#31670=CARTESIAN_POINT('Ctrl Pts',(20.2710606886696,0.657292163719816,4.24771695100806));
#31671=CARTESIAN_POINT('Ctrl Pts',(20.3187765247324,0.147355317357748,4.68736342730055));
#31672=CARTESIAN_POINT('Ctrl Pts',(20.3664923607953,-0.498896366832293,
4.49468216892218));
#31673=CARTESIAN_POINT('Ctrl Pts',(20.4062555575143,-0.653992183610565,
3.9575054511282));
#31674=CARTESIAN_POINT('Ctrl Pts',(20.4380661148895,-0.465699721472375,
3.59327933193152));
#31675=CARTESIAN_POINT('Ctrl Pts',(20.461924032921,-0.215665100260693,3.41899970433759));
#31676=CARTESIAN_POINT('Ctrl Pts',(20.4857819509523,0.0900520562992202,
3.38718375849312));
#31677=CARTESIAN_POINT('Ctrl Pts',(20.5096398689838,0.372154449079436,3.50499792242313));
#31678=CARTESIAN_POINT('Ctrl Pts',(20.5334977870152,0.564103623124681,3.74397162737493));
#31679=CARTESIAN_POINT('Ctrl Pts',(20.5573557050466,0.61766411855396,4.04548854604559));
#31680=CARTESIAN_POINT('Ctrl Pts',(20.581213623078,0.520427284318709,4.33591550271974));
#31681=CARTESIAN_POINT('Ctrl Pts',(20.6050715411094,0.295805552416038,4.5441843692251));
#31682=CARTESIAN_POINT('Ctrl Pts',(20.6289294591409,-0.00108183093298003,
4.61939465531364));
#31683=CARTESIAN_POINT('Ctrl Pts',(20.6527873771723,-0.297740088546312,
4.543141139652));
#31684=CARTESIAN_POINT('Ctrl Pts',(20.6766452952037,-0.521574030203058,
4.33407743490148));
#31685=CARTESIAN_POINT('Ctrl Pts',(20.7005032132351,-0.617878846294169,
4.04332131262121));
#31686=CARTESIAN_POINT('Ctrl Pts',(20.7243611312665,-0.563090193646282,
3.74197268265107));
#31687=CARTESIAN_POINT('Ctrl Pts',(20.748219049298,-0.370613436173077,3.50371837193987));
#31688=CARTESIAN_POINT('Ctrl Pts',(20.7720769673294,-0.0875101228827464,
3.38681864340431));
#31689=CARTESIAN_POINT('Ctrl Pts',(20.7959348853608,0.216991017820888,3.41985835035499));
#31690=CARTESIAN_POINT('Ctrl Pts',(20.8197928033922,0.468432357761717,3.59475855107288));
#31691=CARTESIAN_POINT('Ctrl Pts',(20.8436507214236,0.605329007232586,3.86875129405724));
#31692=CARTESIAN_POINT('Ctrl Pts',(20.8675086394551,0.594206341669864,4.17483793696784));
#31693=CARTESIAN_POINT('Ctrl Pts',(20.8913665574864,0.437783978244149,4.43817193323088));
#31694=CARTESIAN_POINT('Ctrl Pts',(20.9152244755179,0.174311539695801,4.5943609607934));
#31695=CARTESIAN_POINT('Ctrl Pts',(20.9390823935493,-0.13178483570001,4.60521254097096));
#31696=CARTESIAN_POINT('Ctrl Pts',(20.9629403115808,-0.405656219889506,
4.46807317049539));
#31697=CARTESIAN_POINT('Ctrl Pts',(20.9867982296121,-0.580333613298163,
4.21647715910241));
#31698=CARTESIAN_POINT('Ctrl Pts',(21.0106561476436,-0.613103627724174,
3.91194658594648));
#31699=CARTESIAN_POINT('Ctrl Pts',(21.034514065675,-0.495953105920446,3.62894747086441));
#31700=CARTESIAN_POINT('Ctrl Pts',(21.0583719837064,-0.257528539509485,
3.43668080652407));
#31701=CARTESIAN_POINT('Ctrl Pts',(21.0822299017379,0.0438687693677006,
3.38216102944232));
#31702=CARTESIAN_POINT('Ctrl Pts',(21.1060878197692,0.334538969374667,3.47871971028568));
#31703=CARTESIAN_POINT('Ctrl Pts',(21.1299457378007,0.543405278604256,3.7027456213393));
#31704=CARTESIAN_POINT('Ctrl Pts',(21.153803655832,0.619394195209021,3.99945832503004));
#31705=CARTESIAN_POINT('Ctrl Pts',(21.1776615738635,0.543924359096133,4.29630348300169));
#31706=CARTESIAN_POINT('Ctrl Pts',(21.2015194918949,0.33545020099803,4.52069436823682));
#31707=CARTESIAN_POINT('Ctrl Pts',(21.2253774099264,0.0449493312674926,
4.61776129700707));
#31708=CARTESIAN_POINT('Ctrl Pts',(21.2492353279577,-0.256542874348706,
4.56376876117982));
#31709=CARTESIAN_POINT('Ctrl Pts',(21.2730932459892,-0.495303359101402,
4.37191940649105));
#31710=CARTESIAN_POINT('Ctrl Pts',(21.2969511640206,-0.612948680759938,
4.08912562603418));
#31711=CARTESIAN_POINT('Ctrl Pts',(21.320809082052,-0.580711353586496,3.78453820227854));
#31712=CARTESIAN_POINT('Ctrl Pts',(21.3446670000834,-0.406474282201139,
3.53263705712739));
#31713=CARTESIAN_POINT('Ctrl Pts',(21.3685249181149,-0.132843176680646,
3.39501888221951));
#31714=CARTESIAN_POINT('Ctrl Pts',(21.3923828361463,0.17327170411384,3.40533506996376));
#31715=CARTESIAN_POINT('Ctrl Pts',(21.4162407541777,0.437016933425986,3.56106303144932));
#31716=CARTESIAN_POINT('Ctrl Pts',(21.4400986722091,0.593899618413251,3.82412303814848));
#31717=CARTESIAN_POINT('Ctrl Pts',(21.4639565902405,0.605557669197671,4.13018975281259));
#31718=CARTESIAN_POINT('Ctrl Pts',(21.4878145082719,0.469140374803543,4.40442152661638));
#31719=CARTESIAN_POINT('Ctrl Pts',(21.5116724263034,0.218005479642704,4.57976122094124));
#31720=CARTESIAN_POINT('Ctrl Pts',(21.5355303443348,-0.0864376936408111,
4.61333350436739));
#31721=CARTESIAN_POINT('Ctrl Pts',(21.5593882623662,-0.369744496313637,
4.49692903910649));
#31722=CARTESIAN_POINT('Ctrl Pts',(21.5832461803976,-0.562638697999917,
4.2590118877088));
#31723=CARTESIAN_POINT('Ctrl Pts',(21.607104098429,-0.617952412054802,3.95775927442416));
#31724=CARTESIAN_POINT('Ctrl Pts',(21.6309620164605,-0.522159928676552,
3.66683566915707));
#31725=CARTESIAN_POINT('Ctrl Pts',(21.6548199344919,-0.298685119385998,
3.45737981799522));
#31726=CARTESIAN_POINT('Ctrl Pts',(21.6786778525233,-0.00217366238626178,
3.38060938201055));
#31727=CARTESIAN_POINT('Ctrl Pts',(21.7025357705547,0.294869314276287,3.45529682398599));
#31728=CARTESIAN_POINT('Ctrl Pts',(21.7263936885862,0.519808711519421,3.66317902991346));
#31729=CARTESIAN_POINT('Ctrl Pts',(21.7502516066175,0.617640719491047,3.95342313784609));
#31730=CARTESIAN_POINT('Ctrl Pts',(21.774109524649,0.564442747351711,4.25505655730362));
#31731=CARTESIAN_POINT('Ctrl Pts',(21.7979674426804,0.373223148373148,4.49432170089927));
#31732=CARTESIAN_POINT('Ctrl Pts',(21.8218253607118,0.0907403232229101,
4.61271172357229));
#31733=CARTESIAN_POINT('Ctrl Pts',(21.8456832787432,-0.213930982672105,
4.58127703989962));
#31734=CARTESIAN_POINT('Ctrl Pts',(21.8695411967746,-0.466290335940828,
4.40770428630285));
#31735=CARTESIAN_POINT('Ctrl Pts',(21.8933991148061,-0.604629000578284,
4.13443672906324));
#31736=CARTESIAN_POINT('Ctrl Pts',(21.9172570328375,-0.595119404811066,
3.82829572958469));
#31737=CARTESIAN_POINT('Ctrl Pts',(21.9411149508689,-0.440086903840403,
3.56414110135311));
#31738=CARTESIAN_POINT('Ctrl Pts',(21.9649728689003,-0.177441167154219,
3.40656584639871));
#31739=CARTESIAN_POINT('Ctrl Pts',(21.9888307869318,0.128593768301574,3.39410140682164));
#31740=CARTESIAN_POINT('Ctrl Pts',(22.0126887049631,0.403184024583593,3.52979567762293));
#31741=CARTESIAN_POINT('Ctrl Pts',(22.0365466229946,0.579184804342829,3.7804677133541));
#31742=CARTESIAN_POINT('Ctrl Pts',(22.060404541026,0.613559122762511,4.08482137310942));
#31743=CARTESIAN_POINT('Ctrl Pts',(22.0842624590574,0.497901522652627,4.36843389665204));
#31744=CARTESIAN_POINT('Ctrl Pts',(22.1081203770888,0.260493437687466,4.56195429652472));
#31745=CARTESIAN_POINT('Ctrl Pts',(22.1319782951203,-0.0406123884881684,
4.61806156357065));
#31746=CARTESIAN_POINT('Ctrl Pts',(22.1558362131517,-0.33178737942464,4.52303594266224));
#31747=CARTESIAN_POINT('Ctrl Pts',(22.1796941311831,-0.541831318374727,
4.30011378656432));
#31748=CARTESIAN_POINT('Ctrl Pts',(22.2035520492145,-0.619382740812877,
4.00380563470766));
#31749=CARTESIAN_POINT('Ctrl Pts',(22.2274099672459,-0.545478211438426,
3.70656690151735));
#31750=CARTESIAN_POINT('Ctrl Pts',(22.2512678852774,-0.338189400908512,
3.48108055383335));
#31751=CARTESIAN_POINT('Ctrl Pts',(22.2751258033088,-0.0482040696311437,
3.38248414587532));
#31752=CARTESIAN_POINT('Ctrl Pts',(22.2989837213402,0.253568469476171,3.43488718493857));
#31753=CARTESIAN_POINT('Ctrl Pts',(22.3228416393716,0.493336611197201,3.62547570084914));
#31754=CARTESIAN_POINT('Ctrl Pts',(22.346699557403,0.612470512379129,3.90764560936005));
#31755=CARTESIAN_POINT('Ctrl Pts',(22.3705574754344,0.581838691587799,4.21239868278141));
#31756=CARTESIAN_POINT('Ctrl Pts',(22.3944153934659,0.408931458591185,4.46521449128699));
#31757=CARTESIAN_POINT('Ctrl Pts',(22.4182733114973,0.13602935083686,4.60427268703701));
#31758=CARTESIAN_POINT('Ctrl Pts',(22.4421312295287,-0.170135649772668,
4.59556974592947));
#31759=CARTESIAN_POINT('Ctrl Pts',(22.4659891475601,-0.434697828443077,
4.44123378804823));
#31760=CARTESIAN_POINT('Ctrl Pts',(22.4898470655916,-0.592964587096883,
4.17900413283907));
#31761=CARTESIAN_POINT('Ctrl Pts',(22.513704983623,-0.606235276705168,3.87300312362118));
#31762=CARTESIAN_POINT('Ctrl Pts',(22.5375629016543,-0.471265070143009,
3.59805624874041));
#31763=CARTESIAN_POINT('Ctrl Pts',(22.5614208196858,-0.22105744785653,3.4213956854475));
#31764=CARTESIAN_POINT('Ctrl Pts',(22.5852787377172,0.0832042338527798,
3.38621941950615));
#31765=CARTESIAN_POINT('Ctrl Pts',(22.6091366557487,0.36712117327337,3.50112963696785));
#31766=CARTESIAN_POINT('Ctrl Pts',(22.63299457378,0.561265174232679,3.7380264683998));
#31767=CARTESIAN_POINT('Ctrl Pts',(22.6568524918115,0.618167971965146,4.03898443479498));
#31768=CARTESIAN_POINT('Ctrl Pts',(22.6807104098429,0.523905402647805,4.33040686810369));
#31769=CARTESIAN_POINT('Ctrl Pts',(22.7045683278744,0.301545895245711,4.54104106792393));
#31770=CARTESIAN_POINT('Ctrl Pts',(22.7284262459057,0.00542710047790416,
4.61936606261506));
#31771=CARTESIAN_POINT('Ctrl Pts',(22.7522841639372,-0.291974666000346,
4.54625809930836));
#31772=CARTESIAN_POINT('Ctrl Pts',(22.7761420819686,-0.518067845615496,
4.33953802216683));
#31773=CARTESIAN_POINT('Ctrl Pts',(22.7920473606562,-0.584213376873476,
4.14642833911731));
#31774=CARTESIAN_POINT('Ctrl Pts',(22.8,-0.592174260192535,4.04779597854866));
#31775=CARTESIAN_POINT('Ctrl Pts',(3.96816317011931,-0.282716247115855,
3.54616445487434));
#31776=CARTESIAN_POINT('Ctrl Pts',(3.97611580946312,-0.207125539895404,
3.49907532469992));
#31777=CARTESIAN_POINT('Ctrl Pts',(3.99202108815073,-0.0320395462633344,
3.44344227840288));
#31778=CARTESIAN_POINT('Ctrl Pts',(4.01587900618214,0.238586678544665,3.49618207793602));
#31779=CARTESIAN_POINT('Ctrl Pts',(4.03973692421357,0.450798406251909,3.67207593825259));
#31780=CARTESIAN_POINT('Ctrl Pts',(4.06359484224498,0.552814952159096,3.92817792166325));
#31781=CARTESIAN_POINT('Ctrl Pts',(4.0874527602764,0.519633627921064,4.20183097195279));
#31782=CARTESIAN_POINT('Ctrl Pts',(4.11131067830782,0.359398059257131,4.42613686623617));
#31783=CARTESIAN_POINT('Ctrl Pts',(4.13516859633924,0.11127440638865,4.54623750576341));
#31784=CARTESIAN_POINT('Ctrl Pts',(4.15902651437066,-0.164055973910312,
4.53276988152218));
#31785=CARTESIAN_POINT('Ctrl Pts',(4.18288443240208,-0.399271733473279,
4.38902461621758));
#31786=CARTESIAN_POINT('Ctrl Pts',(4.2067423504335,-0.536853866020863,4.15015270818839));
#31787=CARTESIAN_POINT('Ctrl Pts',(4.23060026846491,-0.543161034884179,
3.87456412255522));
#31788=CARTESIAN_POINT('Ctrl Pts',(4.25445818649634,-0.416650307492554,
3.62964815836115));
#31789=CARTESIAN_POINT('Ctrl Pts',(4.27831610452775,-0.188257351244862,
3.47529323740438));
#31790=CARTESIAN_POINT('Ctrl Pts',(4.30217402255918,0.0861697193074588,
3.44924344981891));
#31791=CARTESIAN_POINT('Ctrl Pts',(4.32603194059059,0.339525912432458,3.55786862136322));
#31792=CARTESIAN_POINT('Ctrl Pts',(4.34988985862202,0.509858789389686,3.77460696883261));
#31793=CARTESIAN_POINT('Ctrl Pts',(4.37374777665342,0.555517294574929,4.0464600464808));
#31794=CARTESIAN_POINT('Ctrl Pts',(4.39760569468486,0.465336694276122,4.30695238014399));
#31795=CARTESIAN_POINT('Ctrl Pts',(4.42146361271626,0.261368594047533,4.4923864940975));
#31796=CARTESIAN_POINT('Ctrl Pts',(4.4453215307477,-0.00651124555331369,
4.55741869872598));
#31797=CARTESIAN_POINT('Ctrl Pts',(4.4691794487791,-0.272798909000308,4.48614684730087));
#31798=CARTESIAN_POINT('Ctrl Pts',(4.49303736681053,-0.472379807908186,
4.29599884956661));
#31799=CARTESIAN_POINT('Ctrl Pts',(4.51689528484195,-0.55645097662433,4.03347107014466));
#31800=CARTESIAN_POINT('Ctrl Pts',(4.54075320287336,-0.504454724024634,
3.76275870240323));
#31801=CARTESIAN_POINT('Ctrl Pts',(4.56461112090479,-0.329105550388866,
3.55005829421323));
#31802=CARTESIAN_POINT('Ctrl Pts',(4.5884690389362,-0.0732811049967102,
3.44738088927219));
#31803=CARTESIAN_POINT('Ctrl Pts',(4.61232695696762,0.200462566687888,3.47983390993684));
#31804=CARTESIAN_POINT('Ctrl Pts',(4.63618487499904,0.425187680335341,3.63948170866684));
#31805=CARTESIAN_POINT('Ctrl Pts',(4.66004279303046,0.54594282425631,3.88728604994618));
#31806=CARTESIAN_POINT('Ctrl Pts',(4.68390071106188,0.533200076465109,4.16265202228146));
#31807=CARTESIAN_POINT('Ctrl Pts',(4.7077586290933,0.390075385898422,4.39824514461603));
#31808=CARTESIAN_POINT('Ctrl Pts',(4.73161654712472,0.151566638040082,4.53645648111246));
#31809=CARTESIAN_POINT('Ctrl Pts',(4.75547446515614,-0.124004281411749,
4.54348959519552));
#31810=CARTESIAN_POINT('Ctrl Pts',(4.77933238318755,-0.369252776249408,
4.41762469889406));
#31811=CARTESIAN_POINT('Ctrl Pts',(4.80319030121898,-0.524208909050512,
4.18963918784455));
#31812=CARTESIAN_POINT('Ctrl Pts',(4.82704821925039,-0.550981684424725,
3.91528172969931));
#31813=CARTESIAN_POINT('Ctrl Pts',(4.85090613728181,-0.443024429517375,
3.66164019632193));
#31814=CARTESIAN_POINT('Ctrl Pts',(4.87476405531323,-0.226735633849849,
3.49073685167984));
#31815=CARTESIAN_POINT('Ctrl Pts',(4.89862197334465,0.0449962004486201,
3.44436221885167));
#31816=CARTESIAN_POINT('Ctrl Pts',(4.92247989137607,0.305725238065515,3.53385615878353));
#31817=CARTESIAN_POINT('Ctrl Pts',(4.94633780940749,0.491696127187109,3.73733496539613));
#31818=CARTESIAN_POINT('Ctrl Pts',(4.9701957274389,0.557433919677865,4.00504252782125));
#31819=CARTESIAN_POINT('Ctrl Pts',(4.99405364547033,0.486863934612277,4.27151705483839));
#31820=CARTESIAN_POINT('Ctrl Pts',(5.01791156350174,0.297242455626679,4.47159826597145));
#31821=CARTESIAN_POINT('Ctrl Pts',(5.04176948153317,0.0349370995184326,
4.55636085499566));
#31822=CARTESIAN_POINT('Ctrl Pts',(5.06562739956458,-0.235911329089554,
4.505078060008));
#31823=CARTESIAN_POINT('Ctrl Pts',(5.08948531759601,-0.449073011639563,
4.33028992129829));
#31824=CARTESIAN_POINT('Ctrl Pts',(5.11334323562741,-0.552424110340463,
4.07473689991432));
#31825=CARTESIAN_POINT('Ctrl Pts',(5.13720115365885,-0.520692466332485,
3.80090867070902));
#31826=CARTESIAN_POINT('Ctrl Pts',(5.16105907169026,-0.361637330928202,
3.57576369465428));
#31827=CARTESIAN_POINT('Ctrl Pts',(5.18491698972168,-0.114152017308863,
3.45435605122152));
#31828=CARTESIAN_POINT('Ctrl Pts',(5.2087749077531,0.161246573981014,3.46637321630784));
#31829=CARTESIAN_POINT('Ctrl Pts',(5.23263282578452,0.397215985664045,3.60887666570863));
#31830=CARTESIAN_POINT('Ctrl Pts',(5.25649074381594,0.536055268906009,3.84702042432939));
#31831=CARTESIAN_POINT('Ctrl Pts',(5.28034866184735,0.543814437048104,4.12257185628156));
#31832=CARTESIAN_POINT('Ctrl Pts',(5.30420657987878,0.418596162124088,4.3681511305826));
#31833=CARTESIAN_POINT('Ctrl Pts',(5.32806449791019,0.191019723230217,4.5237074252207));
#31834=CARTESIAN_POINT('Ctrl Pts',(5.35192241594161,-0.0832662412662402,
4.55120298888854));
#31835=CARTESIAN_POINT('Ctrl Pts',(5.37578033397303,-0.337191341646214,
4.44391440730515));
#31836=CARTESIAN_POINT('Ctrl Pts',(5.39963825200445,-0.508663974085987,
4.22807666114996));
#31837=CARTESIAN_POINT('Ctrl Pts',(5.42349617003587,-0.555754409133215,
3.95646795866016));
#31838=CARTESIAN_POINT('Ctrl Pts',(5.4473540880673,-0.466947752701331,3.69550402606682));
#31839=CARTESIAN_POINT('Ctrl Pts',(5.47121200609871,-0.263959651332346,
3.50899765340418));
#31840=CARTESIAN_POINT('Ctrl Pts',(5.49506992413013,0.00357377490351851,
3.44255472911916));
#31841=CARTESIAN_POINT('Ctrl Pts',(5.51892784216155,0.270233315828591,3.51242235806964));
#31842=CARTESIAN_POINT('Ctrl Pts',(5.54278576019296,0.470813450024345,3.70151600181885));
#31843=CARTESIAN_POINT('Ctrl Pts',(5.56664367822439,0.556266870991092,3.96359711366712));
#31844=CARTESIAN_POINT('Ctrl Pts',(5.5905015962558,0.505697889589837,4.23457972281303));
#31845=CARTESIAN_POINT('Ctrl Pts',(5.61435951428722,0.331471999260015,4.4482011999181));
#31846=CARTESIAN_POINT('Ctrl Pts',(5.63821743231864,0.0761921759760934,
4.55222527486821));
#31847=CARTESIAN_POINT('Ctrl Pts',(5.66207535035006,-0.197718709731212,
4.52121522783523));
#31848=CARTESIAN_POINT('Ctrl Pts',(5.68593326838148,-0.423281985227643,
4.3627538599096));
#31849=CARTESIAN_POINT('Ctrl Pts',(5.70979118641289,-0.545341285237878,
4.11558929214995));
#31850=CARTESIAN_POINT('Ctrl Pts',(5.73364910444432,-0.534049786451273,
3.84015999362387));
#31851=CARTESIAN_POINT('Ctrl Pts',(5.75750702247573,-0.392168567195948,
3.6038159310769));
#31852=CARTESIAN_POINT('Ctrl Pts',(5.78136494050716,-0.154391451667357,
3.46434966433946));
#31853=CARTESIAN_POINT('Ctrl Pts',(5.80522285853857,0.121138580962943,3.45586449715393));
#31854=CARTESIAN_POINT('Ctrl Pts',(5.82908077656999,0.367046927720705,3.58043527923202));
#31855=CARTESIAN_POINT('Ctrl Pts',(5.85293869460141,0.523202308305842,3.80760107017232));
#31856=CARTESIAN_POINT('Ctrl Pts',(5.87679661263283,0.551420461789987,4.08181362911724));
#31857=CARTESIAN_POINT('Ctrl Pts',(5.90065453066425,0.44480131269862,4.33602054829434));
#31858=CARTESIAN_POINT('Ctrl Pts',(5.92451244869567,0.229416087376931,4.50806125053784));
#31859=CARTESIAN_POINT('Ctrl Pts',(5.94837036672709,-0.042067546589846,
4.55586721297736));
#31860=CARTESIAN_POINT('Ctrl Pts',(5.97222828475851,-0.30326465903273,4.46774835821298));
#31861=CARTESIAN_POINT('Ctrl Pts',(5.99608620278993,-0.490305038147314,
4.26525255699254));
#31862=CARTESIAN_POINT('Ctrl Pts',(6.01994412082133,-0.557452977205748,
3.99789477357902));
#31863=CARTESIAN_POINT('Ctrl Pts',(6.04380203885278,-0.488287539408226,
3.73105273207384));
#31864=CARTESIAN_POINT('Ctrl Pts',(6.06765995688417,-0.299724270968661,
3.52997381710292));
#31865=CARTESIAN_POINT('Ctrl Pts',(6.09151787491561,-0.0378669053578504,
3.44383251805177));
#31866=CARTESIAN_POINT('Ctrl Pts',(6.11537579294702,0.233243627260218,3.49368287747685));
#31867=CARTESIAN_POINT('Ctrl Pts',(6.13923371097844,0.447331678364145,3.6673537262422));
#31868=CARTESIAN_POINT('Ctrl Pts',(6.16309162900986,0.552012406214274,3.92234268746235));
#31869=CARTESIAN_POINT('Ctrl Pts',(6.18694954704127,0.521753629494025,4.19636433484848));
#31870=CARTESIAN_POINT('Ctrl Pts',(6.2108074650727,0.363831507594212,4.42228768590875));
#31871=CARTESIAN_POINT('Ctrl Pts',(6.23466538310411,0.117094415953721,4.54510476979165));
#31872=CARTESIAN_POINT('Ctrl Pts',(6.25852330113554,-0.158561881267111,
4.53433708369694));
#31873=CARTESIAN_POINT('Ctrl Pts',(6.28238121916695,-0.394905399742298,
4.39345989467659));
#31874=CARTESIAN_POINT('Ctrl Pts',(6.30623913719837,-0.535697351746728,
4.1553358869807));
#31875=CARTESIAN_POINT('Ctrl Pts',(6.33009705522979,-0.543633587309765,
3.88114808171798));
#31876=CARTESIAN_POINT('Ctrl Pts',(6.36190761260502,-0.381130543103143,
3.54983775818315));
#31877=CARTESIAN_POINT('Ctrl Pts',(6.40167080932404,0.0904237977681596,
3.37418170676098));
#31878=CARTESIAN_POINT('Ctrl Pts',(6.4493866453869,0.576013642360818,3.73827828410759));
#31879=CARTESIAN_POINT('Ctrl Pts',(6.49710248144972,0.531303907723303,4.34259299019566));
#31880=CARTESIAN_POINT('Ctrl Pts',(6.54481831751257,-0.000617460830772086,
4.63236849138271));
#31881=CARTESIAN_POINT('Ctrl Pts',(6.5925341535754,-0.532336898979176,4.34139325430452));
#31882=CARTESIAN_POINT('Ctrl Pts',(6.64024998963824,-0.575010046738857,
3.73693099107234));
#31883=CARTESIAN_POINT('Ctrl Pts',(6.68796582570108,-0.0897448725589052,
3.37403863313417));
#31884=CARTESIAN_POINT('Ctrl Pts',(6.73568166176391,0.477988548433368,3.58598174571673));
#31885=CARTESIAN_POINT('Ctrl Pts',(6.78339749782676,0.606749053262868,4.17812127049189));
#31886=CARTESIAN_POINT('Ctrl Pts',(6.83111333388958,0.178337754027021,4.60669083891839));
#31887=CARTESIAN_POINT('Ctrl Pts',(6.87882916995244,-0.413851892207341,
4.47812605548031));
#31888=CARTESIAN_POINT('Ctrl Pts',(6.92654500601527,-0.625990718083913,
3.91049119230943));
#31889=CARTESIAN_POINT('Ctrl Pts',(6.97426084207811,-0.263274891453005,
3.42505341469988));
#31890=CARTESIAN_POINT('Ctrl Pts',(7.02197667814094,0.341211513798207,3.46759805477058));
#31891=CARTESIAN_POINT('Ctrl Pts',(7.06969251420378,0.63235750294684,3.99905552874491));
#31892=CARTESIAN_POINT('Ctrl Pts',(7.11740835026662,0.342800202184808,4.53138035934227));
#31893=CARTESIAN_POINT('Ctrl Pts',(7.16512418632946,-0.261555976381552,
4.57573041153878));
#31894=CARTESIAN_POINT('Ctrl Pts',(7.2128400223923,-0.625721183287191,4.0913783776429));
#31895=CARTESIAN_POINT('Ctrl Pts',(7.26055585845514,-0.41527704940159,3.52311216844965));
#31896=CARTESIAN_POINT('Ctrl Pts',(7.30827169451797,0.176522415171576,3.39277939551711));
#31897=CARTESIAN_POINT('Ctrl Pts',(7.35598753058081,0.606218615784068,3.8200666455489));
#31898=CARTESIAN_POINT('Ctrl Pts',(7.40370336664364,0.479214941044062,4.4125894643569));
#31899=CARTESIAN_POINT('Ctrl Pts',(7.4514192027065,-0.0878591916424711,
4.62622502914213));
#31900=CARTESIAN_POINT('Ctrl Pts',(7.49913503876932,-0.574250874682306,
4.26478851416677));
#31901=CARTESIAN_POINT('Ctrl Pts',(7.54685087483217,-0.53329914461431,3.6601926322252));
#31902=CARTESIAN_POINT('Ctrl Pts',(7.594566710895,-0.00261060360317682,
3.36764708477891));
#31903=CARTESIAN_POINT('Ctrl Pts',(7.64228254695784,0.530475294557976,3.65580094934904));
#31904=CARTESIAN_POINT('Ctrl Pts',(7.68999838302067,0.576417567478113,4.26003809833172));
#31905=CARTESIAN_POINT('Ctrl Pts',(7.73771421908353,0.093026718772369,4.62547826040714));
#31906=CARTESIAN_POINT('Ctrl Pts',(7.78543005514634,-0.475791997136335,
4.41653211173522));
#31907=CARTESIAN_POINT('Ctrl Pts',(7.8331458912092,-0.607683601098078,3.82507811568403));
#31908=CARTESIAN_POINT('Ctrl Pts',(7.88086172727203,-0.181530003744534,
3.39425757752065));
#31909=CARTESIAN_POINT('Ctrl Pts',(7.92857756333487,0.411325389238953,3.51969962646458));
#31910=CARTESIAN_POINT('Ctrl Pts',(7.97629339939771,0.626454348233276,4.08620889879763));
#31911=CARTESIAN_POINT('Ctrl Pts',(8.02400923546054,0.266300640003926,4.57355121287022));
#31912=CARTESIAN_POINT('Ctrl Pts',(8.07172507152339,-0.338401043502061,
4.5341926229444));
#31913=CARTESIAN_POINT('Ctrl Pts',(8.11944090758622,-0.632343841791292,
4.00427672775865));
#31914=CARTESIAN_POINT('Ctrl Pts',(8.16715674364906,-0.345595560302635,
3.47043344766624));
#31915=CARTESIAN_POINT('Ctrl Pts',(8.2148725797119,0.258518441882999,3.42289928101069));
#31916=CARTESIAN_POINT('Ctrl Pts',(8.26258841577473,0.625230981070026,3.90532558443901));
#31917=CARTESIAN_POINT('Ctrl Pts',(8.31030425183758,0.417784289925175,4.47469286043008));
#31918=CARTESIAN_POINT('Ctrl Pts',(8.35802008790041,-0.173320143095541,
4.60814237859973));
#31919=CARTESIAN_POINT('Ctrl Pts',(8.40573592396325,-0.605262021838435,
4.18312539302794));
#31920=CARTESIAN_POINT('Ctrl Pts',(8.45345176002609,-0.481382472773795,
3.58994154129225));
#31921=CARTESIAN_POINT('Ctrl Pts',(8.50116759608892,0.0845580080604409,
3.37332068174828));
#31922=CARTESIAN_POINT('Ctrl Pts',(8.54888343215178,0.572847569000584,3.73218908285563));
#31923=CARTESIAN_POINT('Ctrl Pts',(8.59659926821459,0.535082392934658,4.33699236997728));
#31924=CARTESIAN_POINT('Ctrl Pts',(8.64431510427745,0.00594282213592907,
4.6323303784547));
#31925=CARTESIAN_POINT('Ctrl Pts',(8.69203094034027,-0.528654133672296,
4.34698967074364));
#31926=CARTESIAN_POINT('Ctrl Pts',(8.73974677640312,-0.577779864139828,
3.74300300926635));
#31927=CARTESIAN_POINT('Ctrl Pts',(8.78746261246595,-0.0963214550818077,
3.37502063878676));
#31928=CARTESIAN_POINT('Ctrl Pts',(8.8351784485288,0.473590428273928,3.58096643225285));
#31929=CARTESIAN_POINT('Ctrl Pts',(8.88289428459164,0.608596934220305,4.17171719864135));
#31930=CARTESIAN_POINT('Ctrl Pts',(8.93061012065447,0.184719511004659,4.60477741930878));
#31931=CARTESIAN_POINT('Ctrl Pts',(8.97832595671731,-0.408788681441581,
4.48246123012823));
#31932=CARTESIAN_POINT('Ctrl Pts',(9.02604179278014,-0.626899937697651,
3.91709346970068));
#31933=CARTESIAN_POINT('Ctrl Pts',(9.07375762884299,-0.269319335070538,
3.42786005172794));
#31934=CARTESIAN_POINT('Ctrl Pts',(9.12147346490582,0.335581356962483,3.46403155175812));
#31935=CARTESIAN_POINT('Ctrl Pts',(9.16918930096866,0.632312525313962,3.99239112474344));
#31936=CARTESIAN_POINT('Ctrl Pts',(9.21690513703149,0.348381372290835,4.52773804495445));
#31937=CARTESIAN_POINT('Ctrl Pts',(9.26462097309434,-0.255473755443411,
4.5784549981902));
#31938=CARTESIAN_POINT('Ctrl Pts',(9.31233680915717,-0.624723402584967,
4.09796782591368));
#31939=CARTESIAN_POINT('Ctrl Pts',(9.36005264522002,-0.420279936527615,
3.52751529167185));
#31940=CARTESIAN_POINT('Ctrl Pts',(9.40776848128285,0.170113062081096,3.39095273519949));
#31941=CARTESIAN_POINT('Ctrl Pts',(9.45548431734569,0.604288618254829,3.81368765339017));
#31942=CARTESIAN_POINT('Ctrl Pts',(9.50320015340853,0.483536638109595,4.40751606625661));
#31943=CARTESIAN_POINT('Ctrl Pts',(9.55091598947137,-0.0812544769791981,
4.62711620503893));
#31944=CARTESIAN_POINT('Ctrl Pts',(9.5986318255342,-0.571428355597161,4.27082588331087));
#31945=CARTESIAN_POINT('Ctrl Pts',(9.64634766159704,-0.536850782714826,
3.66583198574659));
#31946=CARTESIAN_POINT('Ctrl Pts',(9.69406349765987,-0.0092748755543832,
3.36770971750703));
#31947=CARTESIAN_POINT('Ctrl Pts',(9.74177933372272,0.52681829253995,3.65022934471732));
#31948=CARTESIAN_POINT('Ctrl Pts',(9.78949516978555,0.579126116453474,4.253948746587));
#31949=CARTESIAN_POINT('Ctrl Pts',(9.83721100584839,0.099613516627068,4.62446310696212));
#31950=CARTESIAN_POINT('Ctrl Pts',(9.88492684191123,-0.471375708268938,
4.42152338761395));
#31951=CARTESIAN_POINT('Ctrl Pts',(9.93264267797408,-0.609493367214024,
3.83149225544889));
#31952=CARTESIAN_POINT('Ctrl Pts',(9.9803585140369,-0.187903888785556,3.39620437793004));
#31953=CARTESIAN_POINT('Ctrl Pts',(10.0280743500997,0.406240621987656,3.51539131074786));
#31954=CARTESIAN_POINT('Ctrl Pts',(10.0757901861626,0.627328118774167,4.07960185956908));
#31955=CARTESIAN_POINT('Ctrl Pts',(10.1235060222254,0.27233055140652,4.57071279591595));
#31956=CARTESIAN_POINT('Ctrl Pts',(10.1712218582883,-0.332752351661881,
4.5377293902281));
#31957=CARTESIAN_POINT('Ctrl Pts',(10.2189376943511,-0.632263650146131,
4.01094081146358));
#31958=CARTESIAN_POINT('Ctrl Pts',(10.2666535304139,-0.351157510074434,
3.47410511718603));
#31959=CARTESIAN_POINT('Ctrl Pts',(10.3143693664768,0.252421974751429,3.42020678572945));
#31960=CARTESIAN_POINT('Ctrl Pts',(10.3620852025396,0.624198476151732,3.89874148420283));
#31961=CARTESIAN_POINT('Ctrl Pts',(10.4098010386024,0.422763912373798,4.47026343579529));
#31962=CARTESIAN_POINT('Ctrl Pts',(10.4575168746653,-0.166901257195935,
4.60993523836389));
#31963=CARTESIAN_POINT('Ctrl Pts',(10.5052327107281,-0.603298434176698,
4.18949412648294));
#31964=CARTESIAN_POINT('Ctrl Pts',(10.552948546791,-0.485677376113382,3.5950376425108));
#31965=CARTESIAN_POINT('Ctrl Pts',(10.6006643828538,0.0779486895418537,
3.3724643225678));
#31966=CARTESIAN_POINT('Ctrl Pts',(10.6483802189166,0.569993274196054,3.72616667108832));
#31967=CARTESIAN_POINT('Ctrl Pts',(10.6960960549795,0.538604264682155,4.3313343790158));
#31968=CARTESIAN_POINT('Ctrl Pts',(10.7438118910423,0.0126066714187673,
4.63223262845832));
#31969=CARTESIAN_POINT('Ctrl Pts',(10.7915277271052,-0.524967822187051,
4.35254192703816));
#31970=CARTESIAN_POINT('Ctrl Pts',(10.839243563168,-0.580456287010268,3.74910654946403));
#31971=CARTESIAN_POINT('Ctrl Pts',(10.8869593992308,-0.102902812003948,
3.37607048800905));
#31972=CARTESIAN_POINT('Ctrl Pts',(10.9346752352937,0.469147898628881,3.5759984978049));
#31973=CARTESIAN_POINT('Ctrl Pts',(10.9823910713565,0.610372875182502,4.16529361116822));
#31974=CARTESIAN_POINT('Ctrl Pts',(11.0301069074193,0.191083048662156,4.60279705802663));
#31975=CARTESIAN_POINT('Ctrl Pts',(11.0778227434822,-0.403681281635282,
4.48674269127424));
#31976=CARTESIAN_POINT('Ctrl Pts',(11.125538579545,-0.627738879572117,3.92370502162571));
#31977=CARTESIAN_POINT('Ctrl Pts',(11.1732544156079,-0.275334205393669,
3.43073020456744));
#31978=CARTESIAN_POINT('Ctrl Pts',(11.2209702516707,0.329914106159097,3.46052459999659));
#31979=CARTESIAN_POINT('Ctrl Pts',(11.2686860877335,0.632197217644931,3.98572755614488));
#31980=CARTESIAN_POINT('Ctrl Pts',(11.3164019237964,0.353923896562866,4.52403711709511));
#31981=CARTESIAN_POINT('Ctrl Pts',(11.3641177598592,-0.24936318455202,4.58111533006939));
#31982=CARTESIAN_POINT('Ctrl Pts',(11.411833595922,-0.623656216347001,4.10454639383227));
#31983=CARTESIAN_POINT('Ctrl Pts',(11.4595494319849,-0.425236148486169,
3.53197089548594));
#31984=CARTESIAN_POINT('Ctrl Pts',(11.5072652680477,0.163684817628688,3.3891937253683));
#31985=CARTESIAN_POINT('Ctrl Pts',(11.5549811041106,0.602291497100466,3.80732935570755));
#31986=CARTESIAN_POINT('Ctrl Pts',(11.6026969401734,0.487804627338989,4.40239740331947));
#31987=CARTESIAN_POINT('Ctrl Pts',(11.6504127762363,-0.0746407375468588,
4.62793772378323));
#31988=CARTESIAN_POINT('Ctrl Pts',(11.6981286122991,-0.568542364648052,
4.276833170433));
#31989=CARTESIAN_POINT('Ctrl Pts',(11.7458444483619,-0.540342790144192,
3.67150845704832));
#31990=CARTESIAN_POINT('Ctrl Pts',(11.7935602844247,-0.0159381172083995,
3.36784258204823));
#31991=CARTESIAN_POINT('Ctrl Pts',(11.8412761204876,0.523102773999324,3.64469659094542));
#31992=CARTESIAN_POINT('Ctrl Pts',(11.8889919565504,0.581770338872691,4.24783118742311));
#31993=CARTESIAN_POINT('Ctrl Pts',(11.9367077926133,0.106189249871976,4.62337859111715));
#31994=CARTESIAN_POINT('Ctrl Pts',(11.9844236286761,-0.466907061217805,
4.4264678426758));
#31995=CARTESIAN_POINT('Ctrl Pts',(12.0321394647389,-0.611235433702689,
3.83792511225401));
#31996=CARTESIAN_POINT('Ctrl Pts',(12.0798553008018,-0.19425690235234,3.39821824509208));
#31997=CARTESIAN_POINT('Ctrl Pts',(12.1275711368646,0.401110731454808,3.51113682306459));
#31998=CARTESIAN_POINT('Ctrl Pts',(12.1752869729275,0.628132208685083,4.07298597854376));
#31999=CARTESIAN_POINT('Ctrl Pts',(12.2230028089903,0.27833021362349,4.56781098689255));
#32000=CARTESIAN_POINT('Ctrl Pts',(12.2707186450531,-0.327066699269377,
4.54120642908287));
#32001=CARTESIAN_POINT('Ctrl Pts',(12.3184344811159,-0.632113229655128,
4.01760367991507));
#32002=CARTESIAN_POINT('Ctrl Pts',(12.3661503171788,-0.356680454936339,
3.47783520061383));
#32003=CARTESIAN_POINT('Ctrl Pts',(12.4138661532416,0.246297469784735,3.4175786911271));
#32004=CARTESIAN_POINT('Ctrl Pts',(12.4615819893045,0.623096638228782,3.89216863128209));
#32005=CARTESIAN_POINT('Ctrl Pts',(12.5092978253673,0.427696576213203,4.46578177652963));
#32006=CARTESIAN_POINT('Ctrl Pts',(12.5570136614302,-0.16046383269669,4.61166034941614));
#32007=CARTESIAN_POINT('Ctrl Pts',(12.604729497493,-0.601267834987779,4.1958418118296));
#32008=CARTESIAN_POINT('Ctrl Pts',(12.6524453335558,-0.489918332714758,
3.60017872502631));
#32009=CARTESIAN_POINT('Ctrl Pts',(12.7001611696187,0.0713307128527425,
3.37167766707246));
#32010=CARTESIAN_POINT('Ctrl Pts',(12.7478770056815,0.56707566724347,3.72017467542775));
#32011=CARTESIAN_POINT('Ctrl Pts',(12.7955928417444,0.542066310823814,4.32563958500381));
#32012=CARTESIAN_POINT('Ctrl Pts',(12.8433086778072,0.0192691204123526,
4.63206465306178));
#32013=CARTESIAN_POINT('Ctrl Pts',(12.89102451387,-0.521223199767296,4.35805502464836));
#32014=CARTESIAN_POINT('Ctrl Pts',(12.9387403499329,-0.583068235550835,
3.7552379577156));
#32015=CARTESIAN_POINT('Ctrl Pts',(12.9864561859957,-0.109472738970043,
3.37718964036075));
#32016=CARTESIAN_POINT('Ctrl Pts',(13.0341720220585,0.464653258261548,3.57107765943178));
#32017=CARTESIAN_POINT('Ctrl Pts',(13.0818878581214,0.612081018822183,4.15885166366515));
#32018=CARTESIAN_POINT('Ctrl Pts',(13.1296036941842,0.197425361721354,4.6007497409078));
#32019=CARTESIAN_POINT('Ctrl Pts',(13.177319530247,-0.398529042827853,4.49097008735187));
#32020=CARTESIAN_POINT('Ctrl Pts',(13.2250353663099,-0.628508095190705,
3.93032504803489));
#32021=CARTESIAN_POINT('Ctrl Pts',(13.2727512023727,-0.281318492899819,
3.4336635891944));
#32022=CARTESIAN_POINT('Ctrl Pts',(13.3204670384356,0.324210210062374,3.45707757060249));
#32023=CARTESIAN_POINT('Ctrl Pts',(13.3681828744984,0.632011688508986,3.97906557286167));
#32024=CARTESIAN_POINT('Ctrl Pts',(13.4158987105612,0.359427108647973,4.52027798167956));
#32025=CARTESIAN_POINT('Ctrl Pts',(13.4636145466241,-0.243224915581421,
4.58371111441534));
#32026=CARTESIAN_POINT('Ctrl Pts',(13.5113303826869,-0.622519757336015,
4.11111334923356));
#32027=CARTESIAN_POINT('Ctrl Pts',(13.5590462187498,-0.430145127231255,
3.53647848575196));
#32028=CARTESIAN_POINT('Ctrl Pts',(13.6067620548126,0.157238391843492,3.38750256099959));
#32029=CARTESIAN_POINT('Ctrl Pts',(13.6544778908755,0.600227476264717,3.8009924589658));
#32030=CARTESIAN_POINT('Ctrl Pts',(13.7021937269383,0.492018433545193,4.39723404398833));
#32031=CARTESIAN_POINT('Ctrl Pts',(13.7499095630011,-0.0680187073756014,
4.62868949418496));
#32032=CARTESIAN_POINT('Ctrl Pts',(13.797625399064,-0.565593222711038,4.28280970824024));
#32033=CARTESIAN_POINT('Ctrl Pts',(13.8453412351268,-0.543774778860562,
3.67722141563181));
#32034=CARTESIAN_POINT('Ctrl Pts',(13.8930570711896,-0.0225995885319848,
3.36804566363559));
#32035=CARTESIAN_POINT('Ctrl Pts',(13.9407729072525,0.519329151684885,3.63920330259016));
#32036=CARTESIAN_POINT('Ctrl Pts',(13.9884887433153,0.584349941003394,4.24168610034696));
#32037=CARTESIAN_POINT('Ctrl Pts',(14.0362045793781,0.112753188118911,4.62222483333648));
#32038=CARTESIAN_POINT('Ctrl Pts',(14.083920415441,-0.462386552345973,4.43136492771341));
#32039=CARTESIAN_POINT('Ctrl Pts',(14.1316362515038,-0.612909607059929,
3.84437597156854));
#32040=CARTESIAN_POINT('Ctrl Pts',(14.1793520875667,-0.200588338784227,
3.40029895531576));
#32041=CARTESIAN_POINT('Ctrl Pts',(14.2270679236295,0.395936287445344,3.50693663598317));
#32042=CARTESIAN_POINT('Ctrl Pts',(14.2747837596923,0.628866528650988,4.06636199058228));
#32043=CARTESIAN_POINT('Ctrl Pts',(14.3224995957552,0.284298960241116,4.5648461081192));
#32044=CARTESIAN_POINT('Ctrl Pts',(14.370215431818,-0.321344717859966,4.54462335329573));
#32045=CARTESIAN_POINT('Ctrl Pts',(14.4179312678809,-0.631892597026201,
4.02426459303334));
#32046=CARTESIAN_POINT('Ctrl Pts',(14.4656471039437,-0.362163781425906,
3.48162328362967));
#32047=CARTESIAN_POINT('Ctrl Pts',(14.5133629400065,0.240145607263868,3.41501528911991));
#32048=CARTESIAN_POINT('Ctrl Pts',(14.5610787760693,0.6219255896881,3.8856077557581));
#32049=CARTESIAN_POINT('Ctrl Pts',(14.6087946121322,0.432581733546503,4.46124838043455));
#32050=CARTESIAN_POINT('Ctrl Pts',(14.656510448195,-0.154008584636381,4.61331752013935));
#32051=CARTESIAN_POINT('Ctrl Pts',(14.7042262842579,-0.599170449821005,
4.20216774399712));
#32052=CARTESIAN_POINT('Ctrl Pts',(14.7519421203207,-0.494104871512583,
3.60536421779174));
#32053=CARTESIAN_POINT('Ctrl Pts',(14.7996579563836,0.0647048130865326,
3.37096080264023));
#32054=CARTESIAN_POINT('Ctrl Pts',(14.8473737924464,0.564095072216763,3.71421376143635));
#32055=CARTESIAN_POINT('Ctrl Pts',(14.8950896285093,0.545468146811986,4.319908620492));
#32056=CARTESIAN_POINT('Ctrl Pts',(14.942805464572,0.0259294290834894,4.63182647092298));
#32057=CARTESIAN_POINT('Ctrl Pts',(14.9905213006349,-0.517420682347921,
4.36352835120552));
#32058=CARTESIAN_POINT('Ctrl Pts',(15.0382371366977,-0.585615419638682,
3.76139655297334));
#32059=CARTESIAN_POINT('Ctrl Pts',(15.0859529727606,-0.116030506223773,
3.3783779715317));
#32060=CARTESIAN_POINT('Ctrl Pts',(15.1336688088234,0.460107006415252,3.56620446371685));
#32061=CARTESIAN_POINT('Ctrl Pts',(15.1813846448862,0.613721175406852,4.15239207167311));
#32062=CARTESIAN_POINT('Ctrl Pts',(15.2291004809491,0.203745745708236,4.59863569535852));
#32063=CARTESIAN_POINT('Ctrl Pts',(15.2768163170119,-0.393332537305518,
4.49514294880206));
#32064=CARTESIAN_POINT('Ctrl Pts',(15.3245321530748,-0.629207499112597,
3.93695281360709));
#32065=CARTESIAN_POINT('Ctrl Pts',(15.3722479891376,-0.287271532882751,
3.43665987978239));
#32066=CARTESIAN_POINT('Ctrl Pts',(15.4199638252004,0.318470302234025,3.45369084645546));
#32067=CARTESIAN_POINT('Ctrl Pts',(15.4676796612633,0.631755958513824,3.97240591487529));
#32068=CARTESIAN_POINT('Ctrl Pts',(15.5153954973261,0.364890397275464,4.51646105625472));
#32069=CARTESIAN_POINT('Ctrl Pts',(15.563111333389,-0.237059630341402,4.58624206290064));
#32070=CARTESIAN_POINT('Ctrl Pts',(15.6108271694518,-0.621314151784485,
4.11766796269128));
#32071=CARTESIAN_POINT('Ctrl Pts',(15.6585430055147,-0.435006327496808,
3.54103756178819));
#32072=CARTESIAN_POINT('Ctrl Pts',(15.7062588415774,0.150774500763906,3.38587942993986));
#32073=CARTESIAN_POINT('Ctrl Pts',(15.7539746776403,0.598096785009218,3.79467766703735));
#32074=CARTESIAN_POINT('Ctrl Pts',(15.8016905137032,0.496177588678611,4.39202656178461));
#32075=CARTESIAN_POINT('Ctrl Pts',(15.849406349766,-0.0613891220090978,
4.62937143274106));
#32076=CARTESIAN_POINT('Ctrl Pts',(15.8971221858288,-0.562581257362808,
4.28875483288714));
#32077=CARTESIAN_POINT('Ctrl Pts',(15.9448380218917,-0.547146367654922,
3.68297022692873));
#32078=CARTESIAN_POINT('Ctrl Pts',(15.9925538579545,-0.0292585496004989,
3.36831893971177));
#32079=CARTESIAN_POINT('Ctrl Pts',(16.0402696940173,0.515497844752703,3.63375008981994));
#32080=CARTESIAN_POINT('Ctrl Pts',(16.0879855300802,0.586864636315616,4.23551416792571));
#32081=CARTESIAN_POINT('Ctrl Pts',(16.135701366143,0.119304602276749,4.62100196177401));
#32082=CARTESIAN_POINT('Ctrl Pts',(16.1834172022059,-0.457814683770117,
4.43621409878185));
#32083=CARTESIAN_POINT('Ctrl Pts',(16.2311330382687,-0.614515701326505,
3.85084411686165));
#32084=CARTESIAN_POINT('Ctrl Pts',(16.2788488743316,-0.206897494815317,
3.40244627748567));
#32085=CARTESIAN_POINT('Ctrl Pts',(16.3265647103943,0.390717864711932,3.50279121604045));
#32086=CARTESIAN_POINT('Ctrl Pts',(16.3742805464572,0.629530997107116,4.05973063144581));
#32087=CARTESIAN_POINT('Ctrl Pts',(16.42199638252,0.290236128279341,4.56181848892059));
#32088=CARTESIAN_POINT('Ctrl Pts',(16.4697122185829,-0.315587043004215,
4.54797978333095));
#32089=CARTESIAN_POINT('Ctrl Pts',(16.5174280546457,-0.631601776766168,
4.03092281095576));
#32090=CARTESIAN_POINT('Ctrl Pts',(16.5651438907086,-0.367606880481235,
3.48546894547127));
#32091=CARTESIAN_POINT('Ctrl Pts',(16.6128597267714,0.233967070508539,3.41251686443844));
#32092=CARTESIAN_POINT('Ctrl Pts',(16.6605755628343,0.620685460604191,3.87905958638177));
#32093=CARTESIAN_POINT('Ctrl Pts',(16.7082913988971,0.437418841753611,4.45666375105816));
#32094=CARTESIAN_POINT('Ctrl Pts',(16.7560072349599,-0.147536230033309,
4.61490656646286));
#32095=CARTESIAN_POINT('Ctrl Pts',(16.8037230710227,-0.597006511643959,
4.20847122033102));
#32096=CARTESIAN_POINT('Ctrl Pts',(16.8514389070856,-0.498236527486006,
3.61059354482716));
#32097=CARTESIAN_POINT('Ctrl Pts',(16.8991547431484,0.058071726216741,3.37031380889701));
#32098=CARTESIAN_POINT('Ctrl Pts',(16.9468705792113,0.561051820186282,3.70828459122417));
#32099=CARTESIAN_POINT('Ctrl Pts',(16.9945864152741,0.548809394786867,4.31414212204871));
#32100=CARTESIAN_POINT('Ctrl Pts',(17.0423022513369,0.0325868576366809,
4.63151810849805));
#32101=CARTESIAN_POINT('Ctrl Pts',(17.0900180873998,-0.513560692294518,
4.3689612987585));
#32102=CARTESIAN_POINT('Ctrl Pts',(17.1377339234626,-0.588097556344686,
3.76758165116972));
#32103=CARTESIAN_POINT('Ctrl Pts',(17.1854497595255,-0.122575385359494,
3.37963534952775));
#32104=CARTESIAN_POINT('Ctrl Pts',(17.2331655955883,0.455509648066065,3.56137945195155));
#32105=CARTESIAN_POINT('Ctrl Pts',(17.2808814316511,0.615293162755707,4.14591555269289));
#32106=CARTESIAN_POINT('Ctrl Pts',(17.328597267714,0.210043498584534,4.59645515619697));
#32107=CARTESIAN_POINT('Ctrl Pts',(17.3763131037768,-0.388092342271454,
4.49926081212312));
#32108=CARTESIAN_POINT('Ctrl Pts',(17.4240289398397,-0.629837013651323,
3.94358758216158));
#32109=CARTESIAN_POINT('Ctrl Pts',(17.4717447759025,-0.293192664107019,
3.43971874351766));
#32110=CARTESIAN_POINT('Ctrl Pts',(17.5194606119653,0.312695020235776,3.45036480373676));
#32111=CARTESIAN_POINT('Ctrl Pts',(17.5671764480282,0.631430056064715,3.96574932190893));
#32112=CARTESIAN_POINT('Ctrl Pts',(17.614892284091,0.370313155609181,4.51258676478657));
#32113=CARTESIAN_POINT('Ctrl Pts',(17.6626081201539,-0.230868013642575,
4.58870789439952));
#32114=CARTESIAN_POINT('Ctrl Pts',(17.7103239562166,-0.620039533605355,
4.12420950615009));
#32115=CARTESIAN_POINT('Ctrl Pts',(17.7580397922796,-0.43981920932378,3.54564761719411));
#32116=CARTESIAN_POINT('Ctrl Pts',(17.8057556283423,0.144293862368219,3.38432451247882));
#32117=CARTESIAN_POINT('Ctrl Pts',(17.8534714644052,0.595899660001039,3.78838568133928));
#32118=CARTESIAN_POINT('Ctrl Pts',(17.901187300468,0.500281630760053,4.38677553513073));
#32119=CARTESIAN_POINT('Ctrl Pts',(17.9489031365309,-0.0547527178302441,
4.62998346370502));
#32120=CARTESIAN_POINT('Ctrl Pts',(17.9966189725937,-0.559506803158163,
4.29466788401745));
#32121=CARTESIAN_POINT('Ctrl Pts',(18.0443348086565,-0.550457182027191,
3.68875425238845));
#32122=CARTESIAN_POINT('Ctrl Pts',(18.0920506447194,-0.0359142607682062,
3.36866237992255));
#32123=CARTESIAN_POINT('Ctrl Pts',(18.1397664807822,0.511609278766163,3.62833755835171));
#32124=CARTESIAN_POINT('Ctrl Pts',(18.187482316845,0.589314145488933,4.22931607570827));
#32125=CARTESIAN_POINT('Ctrl Pts',(18.2351981529079,0.12584276464555,4.61971011226051));
#32126=CARTESIAN_POINT('Ctrl Pts',(18.2829139889707,-0.453191963311679,
4.44101481725822));
#32127=CARTESIAN_POINT('Ctrl Pts',(18.3306298250336,-0.616053538105107,
3.85732882968247));
#32128=CARTESIAN_POINT('Ctrl Pts',(18.3783456610964,-0.213183669654489,
3.40465997308746));
#32129=CARTESIAN_POINT('Ctrl Pts',(18.4260614971592,0.385456042892229,3.49870102369));
#32130=CARTESIAN_POINT('Ctrl Pts',(18.4737773332221,0.630125540247444,4.05309263771424));
#32131=CARTESIAN_POINT('Ctrl Pts',(18.5214931692849,0.296141058265729,4.55872846559028));
#32132=CARTESIAN_POINT('Ctrl Pts',(18.5692090053478,-0.309794314237323,
4.55127534637221));
#32133=CARTESIAN_POINT('Ctrl Pts',(18.6169248414106,-0.631240801177943,
4.0375775941191));
#32134=CARTESIAN_POINT('Ctrl Pts',(18.6646406774734,-0.373009147508776,
3.4893717589807));
#32135=CARTESIAN_POINT('Ctrl Pts',(18.7123565135363,0.227762545801372,3.41008369459593));
#32136=CARTESIAN_POINT('Ctrl Pts',(18.7600723495991,0.619376388724522,3.87252485049244));
#32137=CARTESIAN_POINT('Ctrl Pts',(18.8077881856619,0.442207363551868,4.45202839763978));
#32138=CARTESIAN_POINT('Ctrl Pts',(18.8555040217248,-0.141047487806633,
4.61642731188217));
#32139=CARTESIAN_POINT('Ctrl Pts',(18.9032198577876,-0.594776260815313,
4.21475154067248));
#32140=CARTESIAN_POINT('Ctrl Pts',(18.9509356938505,-0.502312841712761,
3.615866125281));
#32141=CARTESIAN_POINT('Ctrl Pts',(18.9986515299133,0.0514321890198641,
3.36973675771293));
#32142=CARTESIAN_POINT('Ctrl Pts',(19.0463673659762,0.557946249173174,3.70238782336559));
#32143=CARTESIAN_POINT('Ctrl Pts',(19.0940832020389,0.552089683635207,4.30834073020757));
#32144=CARTESIAN_POINT('Ctrl Pts',(19.1417990381018,0.0392406665648073,
4.63113960000379));
#32145=CARTESIAN_POINT('Ctrl Pts',(19.1895148741646,-0.509643658296843,
4.3743532639067));
#32146=CARTESIAN_POINT('Ctrl Pts',(19.2372307102275,-0.590514370077448,
3.77379256516987));
#32147=CARTESIAN_POINT('Ctrl Pts',(19.2849465462903,-0.129106649190522,
3.38096163491845));
#32148=CARTESIAN_POINT('Ctrl Pts',(19.3326623823532,0.450861693465423,3.55660315963506));
#32149=CARTESIAN_POINT('Ctrl Pts',(19.380378218416,0.616796807017627,4.1394228269368));
#32150=CARTESIAN_POINT('Ctrl Pts',(19.4280940544789,0.216317919394901,4.59420836405745));
#32151=CARTESIAN_POINT('Ctrl Pts',(19.4758098905416,-0.382809037079938,
4.50332322288615));
#32152=CARTESIAN_POINT('Ctrl Pts',(19.5235257266046,-0.630396573984801,
3.95022861114352));
#32153=CARTESIAN_POINT('Ctrl Pts',(19.5712415626673,-0.299081219248977,
3.44283985120298));
#32154=CARTESIAN_POINT('Ctrl Pts',(19.6189573987302,0.306884987370396,3.44709979193512));
#32155=CARTESIAN_POINT('Ctrl Pts',(19.666673234793,0.631034051704256,3.95909657101937));
#32156=CARTESIAN_POINT('Ctrl Pts',(19.7143890708559,0.375694716468479,4.50865546647685));
#32157=CARTESIAN_POINT('Ctrl Pts',(19.7621049069187,-0.224650630777236,
4.59110846933868));
#32158=CARTESIAN_POINT('Ctrl Pts',(19.8098207429815,-0.618696275574682,
4.13073699938377));
#32159=CARTESIAN_POINT('Ctrl Pts',(19.8575365790444,-0.44458280157215,3.55030861879767));
#32160=CARTESIAN_POINT('Ctrl Pts',(19.9052524151072,0.13779637220375,3.3828370770856));
#32161=CARTESIAN_POINT('Ctrl Pts',(19.9529682511701,0.593637901716091,3.7821189081517));
#32162=CARTESIAN_POINT('Ctrl Pts',(20.0006840872329,0.504327165075627,4.38147832337345));
#32163=CARTESIAN_POINT('Ctrl Pts',(20.0483999232957,-0.0481046828163007,
4.63053160650705));
#32164=CARTESIAN_POINT('Ctrl Pts',(20.0961157593586,-0.556380679578279,
4.30053671048834));
#32165=CARTESIAN_POINT('Ctrl Pts',(20.1438315954214,-0.553687069357429,
3.69459455385474));
#32166=CARTESIAN_POINT('Ctrl Pts',(20.1915474314843,-0.0426033430871586,
3.36903495876776));
#32167=CARTESIAN_POINT('Ctrl Pts',(20.2392632675471,0.507734449822709,3.62304374442814));
#32168=CARTESIAN_POINT('Ctrl Pts',(20.2869791036099,0.591564791291533,4.22294595084339));
#32169=CARTESIAN_POINT('Ctrl Pts',(20.3346949396728,0.132620199007312,4.618629012875));
#32170=CARTESIAN_POINT('Ctrl Pts',(20.3824107757356,-0.449008129734859,
4.44521533979349));
#32171=CARTESIAN_POINT('Ctrl Pts',(20.4221739724547,-0.588594799935545,
3.96175478680276));
#32172=CARTESIAN_POINT('Ctrl Pts',(20.4539845298298,-0.419131055782338,
3.63395025773895));
#32173=CARTESIAN_POINT('Ctrl Pts',(20.4778424478613,-0.194099195253748,
3.47709810398663));
#32174=CARTESIAN_POINT('Ctrl Pts',(20.5017003658927,0.0810471032980313,
3.44846366347126));
#32175=CARTESIAN_POINT('Ctrl Pts',(20.5255582839241,0.334940048200093,3.55449674151986));
#32176=CARTESIAN_POINT('Ctrl Pts',(20.5494162019556,0.507694843328107,3.76957374638464));
#32177=CARTESIAN_POINT('Ctrl Pts',(20.5732741199869,0.555899439471162,4.04093981905292));
#32178=CARTESIAN_POINT('Ctrl Pts',(20.5971320380184,0.468386015874758,4.30232489481291));
#32179=CARTESIAN_POINT('Ctrl Pts',(20.6209899560498,0.266225827016684,4.48976745893774));
#32180=CARTESIAN_POINT('Ctrl Pts',(20.6448478740812,-0.000973650874560818,
4.55745692740964));
#32181=CARTESIAN_POINT('Ctrl Pts',(20.6687057921126,-0.267966914960919,
4.48882854939535));
#32182=CARTESIAN_POINT('Ctrl Pts',(20.6925637101441,-0.469418090387657,
4.30067062862012));
#32183=CARTESIAN_POINT('Ctrl Pts',(20.7164216281755,-0.556092695039732,
4.03898930289119));
#32184=CARTESIAN_POINT('Ctrl Pts',(20.7402795462069,-0.506782753954552,
3.7677746905255));
#32185=CARTESIAN_POINT('Ctrl Pts',(20.7641374642383,-0.333553132261349,
3.55334514249538));
#32186=CARTESIAN_POINT('Ctrl Pts',(20.7879953822697,-0.0787593560922578,
3.44813505886707));
#32187=CARTESIAN_POINT('Ctrl Pts',(20.8118533003012,0.19529252477751,3.47787088781106));
#32188=CARTESIAN_POINT('Ctrl Pts',(20.8357112183325,0.421590436108717,3.63528155911584));
#32189=CARTESIAN_POINT('Ctrl Pts',(20.859569136364,0.544797804677434,3.8818757964511));
#32190=CARTESIAN_POINT('Ctrl Pts',(20.8834270543954,0.534787374467886,4.15735463375504));
#32191=CARTESIAN_POINT('Ctrl Pts',(20.9072849724269,0.394006808563119,4.39435596913946));
#32192=CARTESIAN_POINT('Ctrl Pts',(20.9311428904582,0.156880874733563,4.53492653211281));
#32193=CARTESIAN_POINT('Ctrl Pts',(20.9550008084897,-0.118606721834374,
4.54469298471526));
#32194=CARTESIAN_POINT('Ctrl Pts',(20.9788587265211,-0.365091735913813,
4.42126716656144));
#32195=CARTESIAN_POINT('Ctrl Pts',(21.0027166445525,-0.522301880015273,
4.19483005048941));
#32196=CARTESIAN_POINT('Ctrl Pts',(21.0265745625839,-0.55179498493052,3.92075168033001));
#32197=CARTESIAN_POINT('Ctrl Pts',(21.0504324806153,-0.446359186657349,
3.66605168284066));
#32198=CARTESIAN_POINT('Ctrl Pts',(21.0742903986468,-0.231776408019839,
3.49301114555638));
#32199=CARTESIAN_POINT('Ctrl Pts',(21.0981483166782,0.0394820154987394,
3.44394319323497));
#32200=CARTESIAN_POINT('Ctrl Pts',(21.1220062347096,0.301086010940692,3.5308462768762));
#32201=CARTESIAN_POINT('Ctrl Pts',(21.145864152741,0.489066275193333,3.73247022529863));
#32202=CARTESIAN_POINT('Ctrl Pts',(21.1697220707724,0.557456513314207,3.9995124910074));
#32203=CARTESIAN_POINT('Ctrl Pts',(21.1935799888039,0.489533449092281,4.26667396594056));
#32204=CARTESIAN_POINT('Ctrl Pts',(21.2174379068352,0.30190612195814,4.46862639215028));
#32205=CARTESIAN_POINT('Ctrl Pts',(21.2412958248667,0.0404545242400231,
4.55598690035157));
#32206=CARTESIAN_POINT('Ctrl Pts',(21.2651537428981,-0.230889306609896,
4.50739346663836));
#32207=CARTESIAN_POINT('Ctrl Pts',(21.2890116609295,-0.445774412697373,
4.33472850921124));
#32208=CARTESIAN_POINT('Ctrl Pts',(21.312869578961,-0.551655532228011,4.08021331346062));
#32209=CARTESIAN_POINT('Ctrl Pts',(21.3367274969923,-0.522641847334507,
3.80608377760199));
#32210=CARTESIAN_POINT('Ctrl Pts',(21.3605854150238,-0.365827994289322,
3.57937204029158));
#32211=CARTESIAN_POINT('Ctrl Pts',(21.3844433330552,-0.119559231686077,
3.45551529680541));
#32212=CARTESIAN_POINT('Ctrl Pts',(21.4083012510867,0.155945019792583,3.46479989471587));
#32213=CARTESIAN_POINT('Ctrl Pts',(21.432159169118,0.393316466074861,3.60495549692644));
#32214=CARTESIAN_POINT('Ctrl Pts',(21.4560170871495,0.534511322676435,3.84171024093472));
#32215=CARTESIAN_POINT('Ctrl Pts',(21.4798750051809,0.545003601087511,4.11717114276091));
#32216=CARTESIAN_POINT('Ctrl Pts',(21.5037329232123,0.422227653432673,4.36398050850424));
#32217=CARTESIAN_POINT('Ctrl Pts',(21.5275908412437,0.196205543263173,4.52178672528827));
#32218=CARTESIAN_POINT('Ctrl Pts',(21.5514487592751,-0.0777941667658609,
4.5520018745543));
#32219=CARTESIAN_POINT('Ctrl Pts',(21.5753066773066,-0.332771083950078,
4.44723752926263));
#32220=CARTESIAN_POINT('Ctrl Pts',(21.5991645953379,-0.506376406606172,
4.23311142556056));
#32221=CARTESIAN_POINT('Ctrl Pts',(21.6230225133694,-0.556158904430687,
3.96198322848119));
#32222=CARTESIAN_POINT('Ctrl Pts',(21.6468804314008,-0.469945400657515,
3.70015116759423));
#32223=CARTESIAN_POINT('Ctrl Pts',(21.6707383494323,-0.268817445367881,
3.51164031394868));
#32224=CARTESIAN_POINT('Ctrl Pts',(21.6945962674636,-0.00195630224560004,
3.44254670619344));
#32225=CARTESIAN_POINT('Ctrl Pts',(21.7184541854951,0.26538321006433,3.50976561349676));
#32226=CARTESIAN_POINT('Ctrl Pts',(21.7423121035264,0.467829298620023,3.6968601820167));
#32227=CARTESIAN_POINT('Ctrl Pts',(21.766170021558,0.555878380248887,3.95808069339639));
#32228=CARTESIAN_POINT('Ctrl Pts',(21.7900279395893,0.508000056083844,4.22955161709966));
#32229=CARTESIAN_POINT('Ctrl Pts',(21.8138858576208,0.335901880562604,4.44489091756156));
#32230=CARTESIAN_POINT('Ctrl Pts',(21.8377437756521,0.0816665454602928,
4.55144227009437));
#32231=CARTESIAN_POINT('Ctrl Pts',(21.8616016936836,-0.192538484559094,
4.52315096660328));
#32232=CARTESIAN_POINT('Ctrl Pts',(21.885459611715,-0.419662610460766,4.36693500143146));
#32233=CARTESIAN_POINT('Ctrl Pts',(21.9093175297464,-0.544167796724789,
4.12099343330092));
#32234=CARTESIAN_POINT('Ctrl Pts',(21.9331754477779,-0.535609133856441,
3.84546567493331));
#32235=CARTESIAN_POINT('Ctrl Pts',(21.9570333658092,-0.396079448060293,
3.60772576847503));
#32236=CARTESIAN_POINT('Ctrl Pts',(21.9808912838407,-0.159697548225882,
3.46590759696012));
#32237=CARTESIAN_POINT('Ctrl Pts',(22.0047492018721,0.115734752223676,3.45468956637345));
#32238=CARTESIAN_POINT('Ctrl Pts',(22.0286071199035,0.362866753203085,3.5768147907664));
#32239=CARTESIAN_POINT('Ctrl Pts',(22.0524650379349,0.521267948732644,3.80242032615069));
#32240=CARTESIAN_POINT('Ctrl Pts',(22.0763229559664,0.552204931742854,4.07633947375325));
#32241=CARTESIAN_POINT('Ctrl Pts',(22.1001808739978,0.448112767182329,4.33159154057792));
#32242=CARTESIAN_POINT('Ctrl Pts',(22.1240387920292,0.23444482469764,4.5057604433585));
#32243=CARTESIAN_POINT('Ctrl Pts',(22.1478967100606,-0.0365512635718279,
4.55625714110116));
#32244=CARTESIAN_POINT('Ctrl Pts',(22.171754628092,-0.298609572266455,4.47073381570218));
#32245=CARTESIAN_POINT('Ctrl Pts',(22.1956125461234,-0.487649706571227,
4.2701032498363));
#32246=CARTESIAN_POINT('Ctrl Pts',(22.2194704641549,-0.557446204325542,
4.00342508191314));
#32247=CARTESIAN_POINT('Ctrl Pts',(22.2433283821863,-0.490931920559466,
3.73590938817905));
#32248=CARTESIAN_POINT('Ctrl Pts',(22.2671863002177,-0.304371409562025,
3.53297104269219));
#32249=CARTESIAN_POINT('Ctrl Pts',(22.2910442182491,-0.0433837978980346,
3.44423399893113));
#32250=CARTESIAN_POINT('Ctrl Pts',(22.3149021362806,0.228212333880327,3.49139688109763));
#32251=CARTESIAN_POINT('Ctrl Pts',(22.3387600543119,0.444004334066149,3.66292708008725));
#32252=CARTESIAN_POINT('Ctrl Pts',(22.3626179723434,0.551225179343846,3.91688078933633));
#32253=CARTESIAN_POINT('Ctrl Pts',(22.3864758903748,0.523656454698273,4.19115941035881));
#32254=CARTESIAN_POINT('Ctrl Pts',(22.4103338084062,0.368039459933637,4.41869434725418));
#32255=CARTESIAN_POINT('Ctrl Pts',(22.4341917264376,0.122426797365049,4.54384711353805));
#32256=CARTESIAN_POINT('Ctrl Pts',(22.458049644469,-0.153122562087755,4.53601444212637));
#32257=CARTESIAN_POINT('Ctrl Pts',(22.4819075625005,-0.391229265084309,
4.39711164706476));
#32258=CARTESIAN_POINT('Ctrl Pts',(22.5057654805319,-0.533669791868601,
4.16110422172694));
#32259=CARTESIAN_POINT('Ctrl Pts',(22.5296233985633,-0.545613449745194,
3.88570245498666));
#32260=CARTESIAN_POINT('Ctrl Pts',(22.5534813165947,-0.424139885198736,
3.63824949626794));
#32261=CARTESIAN_POINT('Ctrl Pts',(22.5773392346261,-0.198952323217499,
3.47925449370713));
#32262=CARTESIAN_POINT('Ctrl Pts',(22.6011971526576,0.0748840438856019,
3.44759575567767));
#32263=CARTESIAN_POINT('Ctrl Pts',(22.625055070689,0.330410085854462,3.55101527375816));
#32264=CARTESIAN_POINT('Ctrl Pts',(22.6489129887204,0.505140231362423,3.7642230866287));
#32265=CARTESIAN_POINT('Ctrl Pts',(22.6727709067518,0.556352908954721,4.03508610068096));
#32266=CARTESIAN_POINT('Ctrl Pts',(22.6966288247833,0.471516332128332,4.29736710820476));
#32267=CARTESIAN_POINT('Ctrl Pts',(22.7204867428146,0.27139215166714,4.48693847894857));
#32268=CARTESIAN_POINT('Ctrl Pts',(22.7443446608461,0.00488440565515616,
4.55743119390072));
#32269=CARTESIAN_POINT('Ctrl Pts',(22.7682025788775,-0.262778018495442,
4.49163382183027));
#32270=CARTESIAN_POINT('Ctrl Pts',(22.7920604969089,-0.466262514422727,
4.30558517247789));
#32271=CARTESIAN_POINT('Ctrl Pts',(22.8079657755965,-0.525793678117208,
4.1317859159904));
#32272=CARTESIAN_POINT('Ctrl Pts',(22.8159184149403,-0.532958495437544,
4.04301651477895));
#32273=CARTESIAN_POINT('Ctrl Pts',(3.98408158505965,-0.251304309929533,
3.59658905474035));
#32274=CARTESIAN_POINT('Ctrl Pts',(3.99203422440346,-0.184112308377066,
3.5547318870523));
#32275=CARTESIAN_POINT('Ctrl Pts',(4.00793950309107,-0.0284797076443847,
3.50528009766423));
#32276=CARTESIAN_POINT('Ctrl Pts',(4.03179742112249,0.212077873916637,3.55216010213054));
#32277=CARTESIAN_POINT('Ctrl Pts',(4.05565533915392,0.400711255741927,3.70851080938071));
#32278=CARTESIAN_POINT('Ctrl Pts',(4.07951325718533,0.49139298320592,3.93615790384083));
#32279=CARTESIAN_POINT('Ctrl Pts',(4.10337117521676,0.461898357851897,4.17940600742409));
#32280=CARTESIAN_POINT('Ctrl Pts',(4.12722909324816,0.319466186301668,4.37878980142624));
#32281=CARTESIAN_POINT('Ctrl Pts',(4.15108701127959,0.0989109688445654,
4.48554634140719));
#32282=CARTESIAN_POINT('Ctrl Pts',(4.174944929311,-0.145828100556353,4.47357507321567));
#32283=CARTESIAN_POINT('Ctrl Pts',(4.19880284734243,-0.354909590370033,
4.34580100620849));
#32284=CARTESIAN_POINT('Ctrl Pts',(4.22266076537384,-0.477205295803391,
4.13346959398438));
#32285=CARTESIAN_POINT('Ctrl Pts',(4.24651868340526,-0.482811689970624,
3.88850100783657));
#32286=CARTESIAN_POINT('Ctrl Pts',(4.27037660143669,-0.370357271909554,
3.67079708031066));
#32287=CARTESIAN_POINT('Ctrl Pts',(4.2942345194681,-0.167340519784032,3.53359217153378));
#32288=CARTESIAN_POINT('Ctrl Pts',(4.31809243749953,0.0765956044913427,
3.51043671457025));
#32289=CARTESIAN_POINT('Ctrl Pts',(4.34195035553093,0.301801986965541,3.60699279882218));
#32290=CARTESIAN_POINT('Ctrl Pts',(4.36580827356237,0.453209578636439,3.79964985833574));
#32291=CARTESIAN_POINT('Ctrl Pts',(4.38966619159377,0.493795074712635,4.04129798000377));
#32292=CARTESIAN_POINT('Ctrl Pts',(4.4135241096252,0.413634228782107,4.27284762322724));
#32293=CARTESIAN_POINT('Ctrl Pts',(4.43738202765661,0.23232854437776,4.43767858897425));
#32294=CARTESIAN_POINT('Ctrl Pts',(4.46123994568804,-0.00578779637616802,
4.49548521832112));
#32295=CARTESIAN_POINT('Ctrl Pts',(4.48509786371945,-0.242488863923451,
4.43213221465579));
#32296=CARTESIAN_POINT('Ctrl Pts',(4.50895578175088,-0.419894798625899,
4.26311111366653));
#32297=CARTESIAN_POINT('Ctrl Pts',(4.53281369978229,-0.494625017545811,
4.02975217827461));
#32298=CARTESIAN_POINT('Ctrl Pts',(4.55667161781372,-0.448405946262215,
3.78911802491887));
#32299=CARTESIAN_POINT('Ctrl Pts',(4.58052953584513,-0.292539406836986,
3.60005025874973));
#32300=CARTESIAN_POINT('Ctrl Pts',(4.60438745387655,-0.0651390137990107,
3.50878109874461));
#32301=CARTESIAN_POINT('Ctrl Pts',(4.62824537190797,0.178189642449287,3.53762834062211));
#32302=CARTESIAN_POINT('Ctrl Pts',(4.65210328993938,0.377946077338085,3.67953804797316));
#32303=CARTESIAN_POINT('Ctrl Pts',(4.67596120797081,0.485284401269169,3.89980943180067));
#32304=CARTESIAN_POINT('Ctrl Pts',(4.69981912600222,0.473957470210434,4.14458013869048));
#32305=CARTESIAN_POINT('Ctrl Pts',(4.72367704403364,0.34673502734182,4.35399706338589));
#32306=CARTESIAN_POINT('Ctrl Pts',(4.74753496206506,0.134726425416229,4.47685206339739));
#32307=CARTESIAN_POINT('Ctrl Pts',(4.77139288009648,-0.110226457398098,
4.48310374471865));
#32308=CARTESIAN_POINT('Ctrl Pts',(4.7952507981279,-0.328225968870003,4.37122340097448));
#32309=CARTESIAN_POINT('Ctrl Pts',(4.81910871615932,-0.465965290257402,
4.16856882376961));
#32310=CARTESIAN_POINT('Ctrl Pts',(4.84296663419074,-0.489763405537152,
3.92469457743051));
#32311=CARTESIAN_POINT('Ctrl Pts',(4.86682455222216,-0.393801027275785,
3.69923455818817));
#32312=CARTESIAN_POINT('Ctrl Pts',(4.89068247025357,-0.201543570920867,
3.54731988215497));
#32313=CARTESIAN_POINT('Ctrl Pts',(4.914540388285,0.039996778460842,3.50609782569371));
#32314=CARTESIAN_POINT('Ctrl Pts',(4.93839830631641,0.271756826018508,3.58564830447545));
#32315=CARTESIAN_POINT('Ctrl Pts',(4.96225622434784,0.437064927107334,3.76651905952651));
#32316=CARTESIAN_POINT('Ctrl Pts',(4.98611414237925,0.495498748108838,4.00448226441646));
#32317=CARTESIAN_POINT('Ctrl Pts',(5.00997206041068,0.432769628082826,4.24134943356216));
#32318=CARTESIAN_POINT('Ctrl Pts',(5.03382997844209,0.26421654558258,4.41920009197534));
#32319=CARTESIAN_POINT('Ctrl Pts',(5.05768789647352,0.031055320573195,4.49454490911931));
#32320=CARTESIAN_POINT('Ctrl Pts',(5.08154581450493,-0.209699776246285,
4.44896002485074));
#32321=CARTESIAN_POINT('Ctrl Pts',(5.10540373253635,-0.399177565666329,
4.29359218508065));
#32322=CARTESIAN_POINT('Ctrl Pts',(5.12926165056777,-0.491045566902382,
4.06643305876778));
#32323=CARTESIAN_POINT('Ctrl Pts',(5.15311956859918,-0.462839551218119,
3.823029239986));
#32324=CARTESIAN_POINT('Ctrl Pts',(5.17697748663061,-0.321456657764784,
3.62289959261435));
#32325=CARTESIAN_POINT('Ctrl Pts',(5.20083540466202,-0.101468855184408,
3.51498126685736));
#32326=CARTESIAN_POINT('Ctrl Pts',(5.22469332269345,0.143330846444675,3.52566323299877));
#32327=CARTESIAN_POINT('Ctrl Pts',(5.24855124072486,0.353082251864168,3.6523334593461));
#32328=CARTESIAN_POINT('Ctrl Pts',(5.27240915875629,0.476495428935435,3.86401762512973));
#32329=CARTESIAN_POINT('Ctrl Pts',(5.2962670767877,0.483392494157105,4.10895318565465));
#32330=CARTESIAN_POINT('Ctrl Pts',(5.32012499481913,0.372086927210194,4.32724672446184));
#32331=CARTESIAN_POINT('Ctrl Pts',(5.34398291285054,0.169795971115995,4.46551952511629));
#32332=CARTESIAN_POINT('Ctrl Pts',(5.36784083088196,-0.0740147250654609,
4.48996012138256));
#32333=CARTESIAN_POINT('Ctrl Pts',(5.39169874891337,-0.299726804847767,
4.39459212172504));
#32334=CARTESIAN_POINT('Ctrl Pts',(5.4155566669448,-0.452147516450583,4.20273559983216));
#32335=CARTESIAN_POINT('Ctrl Pts',(5.43941458497621,-0.494005844030112,
3.96130470137348));
#32336=CARTESIAN_POINT('Ctrl Pts',(5.46327250300764,-0.415066286295368,
3.72933585746768));
#32337=CARTESIAN_POINT('Ctrl Pts',(5.48713042103905,-0.234631715382576,
3.56355176915442));
#32338=CARTESIAN_POINT('Ctrl Pts',(5.51098833907048,0.00317670118048804,
3.50449116189365));
#32339=CARTESIAN_POINT('Ctrl Pts',(5.53484625710188,0.240208327774024,3.56659596294035));
#32340=CARTESIAN_POINT('Ctrl Pts',(5.55870417513332,0.418502475082003,3.73467985673571));
#32341=CARTESIAN_POINT('Ctrl Pts',(5.58256209316472,0.494461367456411,3.96764175273735));
#32342=CARTESIAN_POINT('Ctrl Pts',(5.60642001119615,0.449510986625754,4.20851612161082));
#32343=CARTESIAN_POINT('Ctrl Pts',(5.63027792922757,0.294642925140636,4.39840261889448));
#32344=CARTESIAN_POINT('Ctrl Pts',(5.65413584725899,0.0677266425295592,
4.49086882357174));
#32345=CARTESIAN_POINT('Ctrl Pts',(5.6779937652904,-0.17575064898472,4.46330422991997));
#32346=CARTESIAN_POINT('Ctrl Pts',(5.70185168332183,-0.376252119531055,
4.32244913183746));
#32347=CARTESIAN_POINT('Ctrl Pts',(5.72570960135325,-0.48474969783608,4.10274643779879));
#32348=CARTESIAN_POINT('Ctrl Pts',(5.74956751938466,-0.474712770918799,
3.85791944074229));
#32349=CARTESIAN_POINT('Ctrl Pts',(5.77342543741608,-0.348595640189148,
3.64783501103505));
#32350=CARTESIAN_POINT('Ctrl Pts',(5.7972833554475,-0.13723738064616,3.52386451312966));
#32351=CARTESIAN_POINT('Ctrl Pts',(5.82114127347893,0.1076791581852,3.5163221129105));
#32352=CARTESIAN_POINT('Ctrl Pts',(5.84499919151033,0.326265206982528,3.62705212841851));
#32353=CARTESIAN_POINT('Ctrl Pts',(5.86885710954176,0.465070530553655,3.82897806268729));
#32354=CARTESIAN_POINT('Ctrl Pts',(5.89271502757317,0.490153431381492,4.07272350923538));
#32355=CARTESIAN_POINT('Ctrl Pts',(5.9165729456046,0.395380485146506,4.29868609559117));
#32356=CARTESIAN_POINT('Ctrl Pts',(5.94043086363601,0.203926205561759,4.45161176009809));
#32357=CARTESIAN_POINT('Ctrl Pts',(5.96428878166744,-0.0373935204432717,
4.49410611450448));
#32358=CARTESIAN_POINT('Ctrl Pts',(5.98814669969885,-0.26956963613406,4.41577793841189));
#32359=CARTESIAN_POINT('Ctrl Pts',(6.01200461773027,-0.435828398698505,
4.23578096933615));
#32360=CARTESIAN_POINT('Ctrl Pts',(6.0358625357617,-0.495515688199628,3.99812868033461));
#32361=CARTESIAN_POINT('Ctrl Pts',(6.0597204537931,-0.434035059498629,3.76093483037113));
#32362=CARTESIAN_POINT('Ctrl Pts',(6.08357837182454,-0.266422612259865,
3.58219732064663));
#32363=CARTESIAN_POINT('Ctrl Pts',(6.10743628985594,-0.0336596025775484,
3.50562697870369));
#32364=CARTESIAN_POINT('Ctrl Pts',(6.13129420788738,0.207328476491996,3.54993858195554));
#32365=CARTESIAN_POINT('Ctrl Pts',(6.15515212591877,0.397629707835022,3.70431327123879));
#32366=CARTESIAN_POINT('Ctrl Pts',(6.17901004395022,0.490679606253205,3.93097100878581));
#32367=CARTESIAN_POINT('Ctrl Pts',(6.20286796198161,0.463782811036945,4.17454675550933));
#32368=CARTESIAN_POINT('Ctrl Pts',(6.22672588001306,0.323407044622774,4.3753682944706));
#32369=CARTESIAN_POINT('Ctrl Pts',(6.25058379804445,0.104084330837213,4.48453946106473));
#32370=CARTESIAN_POINT('Ctrl Pts',(6.27444171607588,-0.140944443623038,
4.4749681472433));
#32371=CARTESIAN_POINT('Ctrl Pts',(6.29829963410731,-0.351028389709017,
4.349743491311));
#32372=CARTESIAN_POINT('Ctrl Pts',(6.32215755213872,-0.476177279109797,
4.13807688197341));
#32373=CARTESIAN_POINT('Ctrl Pts',(6.34601547017014,-0.483231738207782,
3.89435343878414));
#32374=CARTESIAN_POINT('Ctrl Pts',(6.37782602754537,-0.338784024988664,
3.5998542259592));
#32375=CARTESIAN_POINT('Ctrl Pts',(6.41758922426439,0.0803770223010952,
3.44371490521648));
#32376=CARTESIAN_POINT('Ctrl Pts',(6.46530506032724,0.512014121509362,3.7673575683149));
#32377=CARTESIAN_POINT('Ctrl Pts',(6.51302089639006,0.472271980317209,4.30452828893312));
#32378=CARTESIAN_POINT('Ctrl Pts',(6.56073673245292,-0.000548856210248058,
4.56210751581942));
#32379=CARTESIAN_POINT('Ctrl Pts',(6.60845256851575,-0.473190198344468,
4.30346185287483));
#32380=CARTESIAN_POINT('Ctrl Pts',(6.65616840457859,-0.511122033036262,
3.76615996983968));
#32381=CARTESIAN_POINT('Ctrl Pts',(6.70388424064142,-0.0797735308749388,
3.44358772816382));
#32382=CARTESIAN_POINT('Ctrl Pts',(6.75160007670426,0.424880365184703,3.63198234005898));
#32383=CARTESIAN_POINT('Ctrl Pts',(6.7993159127671,0.539334593204737,4.15833063512042));
#32384=CARTESIAN_POINT('Ctrl Pts',(6.84703174882994,0.158523065679302,4.53928284691909));
#32385=CARTESIAN_POINT('Ctrl Pts',(6.89474758489278,-0.367869781963911,
4.42500259414721));
#32386=CARTESIAN_POINT('Ctrl Pts',(6.94246342095561,-0.556438361909488,
3.92043630538129));
#32387=CARTESIAN_POINT('Ctrl Pts',(6.99017925701846,-0.234023037562683,
3.48893437735136));
#32388=CARTESIAN_POINT('Ctrl Pts',(7.03789509308128,0.303300305128555,3.52675198254107));
#32389=CARTESIAN_POINT('Ctrl Pts',(7.08561092914413,0.562097748282813,3.99916046672433));
#32390=CARTESIAN_POINT('Ctrl Pts',(7.13332676520696,0.304712478085684,4.47233993757656));
#32391=CARTESIAN_POINT('Ctrl Pts',(7.18104260126981,-0.232495107101315,
4.51176235979777));
#32392=CARTESIAN_POINT('Ctrl Pts',(7.22875843733264,-0.556198774489988,
4.08122554105153));
#32393=CARTESIAN_POINT('Ctrl Pts',(7.27647427339549,-0.369136593294786,
3.57609805363465));
#32394=CARTESIAN_POINT('Ctrl Pts',(7.32419010945832,0.156909424853758,3.46024624852207));
#32395=CARTESIAN_POINT('Ctrl Pts',(7.37190594552116,0.538863091386428,3.84005861730642));
#32396=CARTESIAN_POINT('Ctrl Pts',(7.41962178158399,0.425970496197337,4.36674761950234));
#32397=CARTESIAN_POINT('Ctrl Pts',(7.46733761764684,-0.0780973635293338,
4.55664663921719));
#32398=CARTESIAN_POINT('Ctrl Pts',(7.51505345370967,-0.510447210801067,
4.2353684852172));
#32399=CARTESIAN_POINT('Ctrl Pts',(7.56276928977251,-0.474045531130633,
3.69794782953315));
#32400=CARTESIAN_POINT('Ctrl Pts',(7.61048512583535,-0.00232054557778912,
3.43790632971152));
#32401=CARTESIAN_POINT('Ctrl Pts',(7.65820096189818,0.471535432411473,3.69404409621074));
#32402=CARTESIAN_POINT('Ctrl Pts',(7.70591679796103,0.512373167457076,4.23114587691112));
#32403=CARTESIAN_POINT('Ctrl Pts',(7.75363263402387,0.0826907388754792,
4.55598284219971));
#32404=CARTESIAN_POINT('Ctrl Pts',(7.80134847008669,-0.422927867535356,
4.3702522086048));
#32405=CARTESIAN_POINT('Ctrl Pts',(7.84906430614955,-0.540165305628305,
3.84451327478339));
#32406=CARTESIAN_POINT('Ctrl Pts',(7.89678014221237,-0.161360632039799,
3.46156019320034));
#32407=CARTESIAN_POINT('Ctrl Pts',(7.94449597827521,0.365623992797271,3.57306467116217));
#32408=CARTESIAN_POINT('Ctrl Pts',(7.99221181433806,0.556850479203549,4.07663043084052));
#32409=CARTESIAN_POINT('Ctrl Pts',(8.03992765040089,0.236712602309549,4.50982528676712));
#32410=CARTESIAN_POINT('Ctrl Pts',(8.08764348646373,-0.300802099575971,
4.47483973718518));
#32411=CARTESIAN_POINT('Ctrl Pts',(8.13535932252656,-0.562085604986122,
4.00380155059756));
#32412=CARTESIAN_POINT('Ctrl Pts',(8.18307515858941,-0.307197250538534,
3.52927234160183));
#32413=CARTESIAN_POINT('Ctrl Pts',(8.23079099465223,0.229795065915734,3.48701958438918));
#32414=CARTESIAN_POINT('Ctrl Pts',(8.27850683071509,0.555763037488074,3.91584463605021));
#32415=CARTESIAN_POINT('Ctrl Pts',(8.32622266677791,0.371365260221553,4.42195085332305));
#32416=CARTESIAN_POINT('Ctrl Pts',(8.37393850284076,-0.154062949695418,
4.54057310944092));
#32417=CARTESIAN_POINT('Ctrl Pts',(8.4216543389036,-0.538012782343907,4.16277876137275));
#32418=CARTESIAN_POINT('Ctrl Pts',(8.46937017496643,-0.427897198575242,
3.6355021720628));
#32419=CARTESIAN_POINT('Ctrl Pts',(8.51708601102927,0.0751629666897603,
3.44294954666756));
#32420=CARTESIAN_POINT('Ctrl Pts',(8.56480184709211,0.50919982311266,3.76194492389047));
#32421=CARTESIAN_POINT('Ctrl Pts',(8.61251768315494,0.475630646924824,4.29954994045293));
#32422=CARTESIAN_POINT('Ctrl Pts',(8.66023351921779,0.00528252914771292,
4.56207363752918));
#32423=CARTESIAN_POINT('Ctrl Pts',(8.70794935528062,-0.469916616427902,
4.30843646464781));
#32424=CARTESIAN_POINT('Ctrl Pts',(8.75566519134346,-0.513584102541225,
3.7715573403753));
#32425=CARTESIAN_POINT('Ctrl Pts',(8.8033810274063,-0.0856194047837525,
3.44446062547832));
#32426=CARTESIAN_POINT('Ctrl Pts',(8.85109686346913,0.420970909810523,3.6275242662766));
#32427=CARTESIAN_POINT('Ctrl Pts',(8.89881269953199,0.540977160455745,4.15263810462895));
#32428=CARTESIAN_POINT('Ctrl Pts',(8.9465285355948,0.1641957606509,4.5375820228614));
#32429=CARTESIAN_POINT('Ctrl Pts',(8.99424437165766,-0.363369132636193,
4.42885609773758));
#32430=CARTESIAN_POINT('Ctrl Pts',(9.04196020772048,-0.557246560270691,
3.92630501926208));
#32431=CARTESIAN_POINT('Ctrl Pts',(9.08967604378333,-0.239395897268157,
3.49142917554125));
#32432=CARTESIAN_POINT('Ctrl Pts',(9.13739187984617,0.298295701775085,3.52358174528888));
#32433=CARTESIAN_POINT('Ctrl Pts',(9.18510771590899,0.562057768008922,3.99323652897485));
#32434=CARTESIAN_POINT('Ctrl Pts',(9.23282355197185,0.309673537509763,4.46910231217259));
#32435=CARTESIAN_POINT('Ctrl Pts',(9.28053938803466,-0.227088667424462,
4.51418422403538));
#32436=CARTESIAN_POINT('Ctrl Pts',(9.32825522409753,-0.555311854854516,
4.08708285122523));
#32437=CARTESIAN_POINT('Ctrl Pts',(9.37597106016035,-0.373583621400482,
3.58001195619306));
#32438=CARTESIAN_POINT('Ctrl Pts',(9.4236868962232,0.151212199908504,3.45862254413551));
#32439=CARTESIAN_POINT('Ctrl Pts',(9.47140273228603,0.537147531342748,3.83438837996121));
#32440=CARTESIAN_POINT('Ctrl Pts',(9.51911856834887,0.429812019667804,4.36223791473086));
#32441=CARTESIAN_POINT('Ctrl Pts',(9.5668344044117,-0.0722264831760907,
4.5574387986564));
#32442=CARTESIAN_POINT('Ctrl Pts',(9.61455024047456,-0.507938295172089,
4.24073505647735));
#32443=CARTESIAN_POINT('Ctrl Pts',(9.66226607653738,-0.477202555076283,
3.70296060775017));
#32444=CARTESIAN_POINT('Ctrl Pts',(9.70998191260023,-0.00824436594879979,
3.43796200346455));
#32445=CARTESIAN_POINT('Ctrl Pts',(9.75769774866306,0.46828475128534,3.68909153946361));
#32446=CARTESIAN_POINT('Ctrl Pts',(9.80541358472589,0.514780775927077,4.22573309871483));
#32447=CARTESIAN_POINT('Ctrl Pts',(9.85312942078874,0.0885456931146035,
4.55508048006603));
#32448=CARTESIAN_POINT('Ctrl Pts',(9.90084525685159,-0.419002262135622,
4.37468891556157));
#32449=CARTESIAN_POINT('Ctrl Pts',(9.9485610929144,-0.541773992888202,3.8502147545669));
#32450=CARTESIAN_POINT('Ctrl Pts',(9.99627692897727,-0.167026329707142,
3.46329068919569));
#32451=CARTESIAN_POINT('Ctrl Pts',(10.0439927650401,0.361104182074418,3.56923504227033));
#32452=CARTESIAN_POINT('Ctrl Pts',(10.0917086011029,0.557627167155001,4.07075748419897));
#32453=CARTESIAN_POINT('Ctrl Pts',(10.1394244371657,0.242072544440304,4.50730223964386));
#32454=CARTESIAN_POINT('Ctrl Pts',(10.1871402732286,-0.295781020598791,
4.47798354257549));
#32455=CARTESIAN_POINT('Ctrl Pts',(10.2348561092914,-0.56201432324602,4.00972520363789));
#32456=CARTESIAN_POINT('Ctrl Pts',(10.2825719453543,-0.312141225154507,
3.53253606055812));
#32457=CARTESIAN_POINT('Ctrl Pts',(10.3302877814171,0.224375962906492,3.48462624592509));
#32458=CARTESIAN_POINT('Ctrl Pts',(10.37800361748,0.554845251762499,3.90999207970357));
#32459=CARTESIAN_POINT('Ctrl Pts',(10.4257194535428,0.375791608533427,4.41801357164013));
#32460=CARTESIAN_POINT('Ctrl Pts',(10.4734352896056,-0.148357251109035,
4.54216676877402));
#32461=CARTESIAN_POINT('Ctrl Pts',(10.5211511256685,-0.536267364288337,
4.16843987983467));
#32462=CARTESIAN_POINT('Ctrl Pts',(10.5688669617313,-0.431714905307627,
3.64003205746247));
#32463=CARTESIAN_POINT('Ctrl Pts',(10.6165827977942,0.0692879940047382,
3.44218833554121));
#32464=CARTESIAN_POINT('Ctrl Pts',(10.664298633857,0.50666266228973,3.75659164812817));
#32465=CARTESIAN_POINT('Ctrl Pts',(10.7120144699198,0.478761211786921,4.29452059555793));
#32466=CARTESIAN_POINT('Ctrl Pts',(10.7597303059827,0.0112059738120427,
4.56198674830498));
#32467=CARTESIAN_POINT('Ctrl Pts',(10.8074461420455,-0.466639882340508,
4.31337182280594));
#32468=CARTESIAN_POINT('Ctrl Pts',(10.8551619781083,-0.515963154362253,
3.77698273057893));
#32469=CARTESIAN_POINT('Ctrl Pts',(10.9028778141712,-0.0914695226195351,
3.44539382842306));
#32470=CARTESIAN_POINT('Ctrl Pts',(10.950593650234,0.417021979184216,3.62310830733915));
#32471=CARTESIAN_POINT('Ctrl Pts',(10.9983094862969,0.542555780795161,4.14692822684982));
#32472=CARTESIAN_POINT('Ctrl Pts',(11.0460253223597,0.169852260608159,4.53582169486292));
#32473=CARTESIAN_POINT('Ctrl Pts',(11.0937411584225,-0.358829204008283,
4.43266185580689));
#32474=CARTESIAN_POINT('Ctrl Pts',(11.1414569944853,-0.55799228928692,3.93218197720501));
#32475=CARTESIAN_POINT('Ctrl Pts',(11.1891728305482,-0.244742469498405,
3.49398043245019));
#32476=CARTESIAN_POINT('Ctrl Pts',(11.236888666611,0.293258125877444,3.5204644426882));
#32477=CARTESIAN_POINT('Ctrl Pts',(11.2846045026739,0.561955271903759,3.98731333380864));
#32478=CARTESIAN_POINT('Ctrl Pts',(11.3323203387367,0.314600244947554,4.46581258570203));
#32479=CARTESIAN_POINT('Ctrl Pts',(11.3800361747996,-0.221657027690976,
4.51654897269734));
#32480=CARTESIAN_POINT('Ctrl Pts',(11.4277520108624,-0.554363241169119,
4.0929304899371));
#32481=CARTESIAN_POINT('Ctrl Pts',(11.4754678469252,-0.377989160306769,
3.58397250834823));
#32482=CARTESIAN_POINT('Ctrl Pts',(11.5231836829881,0.145498182576105,3.45705897374896));
#32483=CARTESIAN_POINT('Ctrl Pts',(11.5708995190509,0.535372305622036,3.82873653777755));
#32484=CARTESIAN_POINT('Ctrl Pts',(11.6186153551137,0.43360580265347,4.35768797439208));
#32485=CARTESIAN_POINT('Ctrl Pts',(11.6663311911766,-0.0663475807746441,
4.55816904038548));
#32486=CARTESIAN_POINT('Ctrl Pts',(11.7140470272394,-0.505372959888646,
4.24607488805821));
#32487=CARTESIAN_POINT('Ctrl Pts',(11.7617628633023,-0.480306573774387,
3.70800637967828));
#32488=CARTESIAN_POINT('Ctrl Pts',(11.8094786993651,-0.0141672704965164,
3.43808010573911));
#32489=CARTESIAN_POINT('Ctrl Pts',(11.8571945354279,0.464982055269784,3.68417351694868));
#32490=CARTESIAN_POINT('Ctrl Pts',(11.9049103714908,0.517131205013274,4.22029524715934));
#32491=CARTESIAN_POINT('Ctrl Pts',(11.9526262075536,0.0943908121067024,
4.55411646222552));
#32492=CARTESIAN_POINT('Ctrl Pts',(12.0003420436165,-0.415030115946784,
4.37908400385228));
#32493=CARTESIAN_POINT('Ctrl Pts',(12.0480578796793,-0.543322502467158,
3.85593287178435));
#32494=CARTESIAN_POINT('Ctrl Pts',(12.0957737157421,-0.172673474880652,
3.46508080031456));
#32495=CARTESIAN_POINT('Ctrl Pts',(12.143489551805,0.356544261611682,3.56545326070575));
#32496=CARTESIAN_POINT('Ctrl Pts',(12.1912053878678,0.558341916527368,4.06487667815191));
#32497=CARTESIAN_POINT('Ctrl Pts',(12.2389212239306,0.247405598301292,4.50472284379514));
#32498=CARTESIAN_POINT('Ctrl Pts',(12.2866370599935,-0.290727087669313,
4.48107425582212));
#32499=CARTESIAN_POINT('Ctrl Pts',(12.3343528960563,-0.56188061562194,4.01564777644873));
#32500=CARTESIAN_POINT('Ctrl Pts',(12.3820687321191,-0.317050528604376,
3.5358517031905));
#32501=CARTESIAN_POINT('Ctrl Pts',(12.429784568182,0.218931937280033,3.48229015273196));
#32502=CARTESIAN_POINT('Ctrl Pts',(12.4775004042448,0.553865836459325,3.90414952100961));
#32503=CARTESIAN_POINT('Ctrl Pts',(12.5252162403077,0.380176215696692,4.4140298589933));
#32504=CARTESIAN_POINT('Ctrl Pts',(12.5729320763705,-0.142635073703209,
4.54370020679522));
#32505=CARTESIAN_POINT('Ctrl Pts',(12.6206479124333,-0.53446238019874,4.17408228879405));
#32506=CARTESIAN_POINT('Ctrl Pts',(12.6683637484962,-0.435484659196984,
3.644601926393));
#32507=CARTESIAN_POINT('Ctrl Pts',(12.716079584559,0.0634053251381518,3.44148908348752));
#32508=CARTESIAN_POINT('Ctrl Pts',(12.7637954206219,0.504069223782589,3.75126540901054));
#32509=CARTESIAN_POINT('Ctrl Pts',(12.8115112566847,0.481838598125516,4.2894585367128));
#32510=CARTESIAN_POINT('Ctrl Pts',(12.8592270927475,0.0171281737699642,
4.56183743625962));
#32511=CARTESIAN_POINT('Ctrl Pts',(12.9069429288104,-0.463311316109371,
4.31827237310907));
#32512=CARTESIAN_POINT('Ctrl Pts',(12.9546587648732,-0.518284895444539,
3.78243289248252));
#32513=CARTESIAN_POINT('Ctrl Pts',(13.0023746009361,-0.0973094804548018,
3.44638863438952));
#32514=CARTESIAN_POINT('Ctrl Pts',(13.0500904369989,0.413026727735397,3.61873421174243));
#32515=CARTESIAN_POINT('Ctrl Pts',(13.0978062730617,0.544074136613086,4.14120202898048));
#32516=CARTESIAN_POINT('Ctrl Pts',(13.1455221091246,0.17548989418231,4.53400185033327));
#32517=CARTESIAN_POINT('Ctrl Pts',(13.1932379451874,-0.354249418335187,
4.4364195558504));
#32518=CARTESIAN_POINT('Ctrl Pts',(13.2409537812502,-0.558676039167545,
3.93806646805208));
#32519=CARTESIAN_POINT('Ctrl Pts',(13.2886696173131,-0.250061856896528,
3.49658789561142));
#32520=CARTESIAN_POINT('Ctrl Pts',(13.3363854533759,0.288187976258808,3.51740040462167));
#32521=CARTESIAN_POINT('Ctrl Pts',(13.3841012894388,0.56179035647369,3.9813915478171));
#32522=CARTESIAN_POINT('Ctrl Pts',(13.4318171255016,0.319492008083037,4.46247111897993));
#32523=CARTESIAN_POINT('Ctrl Pts',(13.4795329615644,-0.21620076734671,4.51885634555065));
#32524=CARTESIAN_POINT('Ctrl Pts',(13.5272487976273,-0.553353051445561,
4.09876780637113));
#32525=CARTESIAN_POINT('Ctrl Pts',(13.5749646336901,-0.382352713970831,
3.58797927086295));
#32526=CARTESIAN_POINT('Ctrl Pts',(13.6226804697529,0.139768003996038,3.45555571067516));
#32527=CARTESIAN_POINT('Ctrl Pts',(13.6703963058158,0.53353761328617,3.82310371872654));
#32528=CARTESIAN_POINT('Ctrl Pts',(13.7181121418786,0.437351422764197,4.35309830377052));
#32529=CARTESIAN_POINT('Ctrl Pts',(13.7658279779415,-0.0604613087987784,
4.55883728334624));
#32530=CARTESIAN_POINT('Ctrl Pts',(13.8135438140043,-0.502751490175015,
4.25138738680826));
#32531=CARTESIAN_POINT('Ctrl Pts',(13.8612596500671,-0.483357242297515,
3.71308458487209));
#32532=CARTESIAN_POINT('Ctrl Pts',(13.90897548613,-0.0200886014110514,3.43826062340902));
#32533=CARTESIAN_POINT('Ctrl Pts',(13.9566913221928,0.461627711254046,3.67929057494076));
#32534=CARTESIAN_POINT('Ctrl Pts',(14.0044071582557,0.519424193619207,4.21483292625321));
#32535=CARTESIAN_POINT('Ctrl Pts',(14.0521229943185,0.100225446615308,4.55309089575788));
#32536=CARTESIAN_POINT('Ctrl Pts',(14.0998388303813,-0.411011870182152,
4.38343698529073));
#32537=CARTESIAN_POINT('Ctrl Pts',(14.1475546664441,-0.544810662360815,
3.86166699129474));
#32538=CARTESIAN_POINT('Ctrl Pts',(14.195270502507,-0.178301440303968,3.46693032771971));
#32539=CARTESIAN_POINT('Ctrl Pts',(14.2429863385698,0.351944737904315,3.5617197465309));
#32540=CARTESIAN_POINT('Ctrl Pts',(14.2907021746327,0.558994647929194,4.05898866591129));
#32541=CARTESIAN_POINT('Ctrl Pts',(14.3384180106955,0.252711171522458,4.50208738572805));
#32542=CARTESIAN_POINT('Ctrl Pts',(14.3861338467583,-0.28564086215454,4.48411153362329));
#32543=CARTESIAN_POINT('Ctrl Pts',(14.4338496828212,-0.561684496965419,
4.02156861117883));
#32544=CARTESIAN_POINT('Ctrl Pts',(14.481565518884,-0.321924615586062,3.53921890121312));
#32545=CARTESIAN_POINT('Ctrl Pts',(14.5292813549469,0.213463593732893,3.48001156429194));
#32546=CARTESIAN_POINT('Ctrl Pts',(14.5769971910097,0.552824900367352,3.89831760893199));
#32547=CARTESIAN_POINT('Ctrl Pts',(14.6247130270725,0.384518594689996,4.4100001578745));
#32548=CARTESIAN_POINT('Ctrl Pts',(14.6724288631354,-0.136897053070264,
4.54517325317752));
#32549=CARTESIAN_POINT('Ctrl Pts',(14.7201446991982,-0.532598030564186,
4.17970536151887));
#32550=CARTESIAN_POINT('Ctrl Pts',(14.7678605352611,-0.439206041516937,
3.64921127125505));
#32551=CARTESIAN_POINT('Ctrl Pts',(14.8155763713239,0.0575156135089261,
3.44085186817608));
#32552=CARTESIAN_POINT('Ctrl Pts',(14.8632922073868,0.501419795658073,3.74596679815093));
#32553=CARTESIAN_POINT('Ctrl Pts',(14.9110080434496,0.484862464119148,4.284364326187));
#32554=CARTESIAN_POINT('Ctrl Pts',(14.9587238795124,0.0230484712116303,
4.56162571797798));
#32555=CARTESIAN_POINT('Ctrl Pts',(15.0064397155752,-0.459931287455839,
4.32313757122732));
#32556=CARTESIAN_POINT('Ctrl Pts',(15.0541555516381,-0.5205490679001,3.78790722070797));
#32557=CARTESIAN_POINT('Ctrl Pts',(15.1018713877009,-0.103138629614742,
3.44744493287938));
#32558=CARTESIAN_POINT('Ctrl Pts',(15.1495872237638,0.40898559923764,3.61440246534021));
#32559=CARTESIAN_POINT('Ctrl Pts',(15.1973030598266,0.545532059257757,4.13546014705983));
#32560=CARTESIAN_POINT('Ctrl Pts',(15.2450188958894,0.181108035171788,4.53212269141213));
#32561=CARTESIAN_POINT('Ctrl Pts',(15.2927347319523,-0.349630284317748,
4.44012878048063));
#32562=CARTESIAN_POINT('Ctrl Pts',(15.3404505680151,-0.559297733964875,
3.94395783818199));
#32563=CARTESIAN_POINT('Ctrl Pts',(15.3881664040779,-0.255353468610234,
3.49925127540033));
#32564=CARTESIAN_POINT('Ctrl Pts',(15.4358822401408,0.283085816087337,3.51438997142805));
#32565=CARTESIAN_POINT('Ctrl Pts',(15.4835980762036,0.561563040036739,3.97547182876414));
#32566=CARTESIAN_POINT('Ctrl Pts',(15.5313139122665,0.324348283562367,4.45907828316053));
#32567=CARTESIAN_POINT('Ctrl Pts',(15.5790297483293,-0.210720492447169,
4.52110608630326));
#32568=CARTESIAN_POINT('Ctrl Pts',(15.6267455843921,-0.552281397890927,
4.10459415214592));
#32569=CARTESIAN_POINT('Ctrl Pts',(15.674461420455,-0.386673797709831,3.59203179868507));
#32570=CARTESIAN_POINT('Ctrl Pts',(15.7221772565178,0.134022300649356,3.45411292188939));
#32571=CARTESIAN_POINT('Ctrl Pts',(15.7698930925807,0.531643658124066,3.81749054847505));
#32572=CARTESIAN_POINT('Ctrl Pts',(15.8176089286435,0.441048463954279,4.34846941266494));
#32573=CARTESIAN_POINT('Ctrl Pts',(15.8653247647064,-0.054568321067637,
4.5594434533135));
#32574=CARTESIAN_POINT('Ctrl Pts',(15.9130406007692,-0.500074177211609,
4.25667196264028));
#32575=CARTESIAN_POINT('Ctrl Pts',(15.960756436832,-0.486354221791887,3.71819465926869));
#32576=CARTESIAN_POINT('Ctrl Pts',(16.0084722728949,-0.0260077009790528,
3.4385035364232));
#32577=CARTESIAN_POINT('Ctrl Pts',(16.0561881089577,0.458222091822753,3.6744432558139));
#32578=CARTESIAN_POINT('Ctrl Pts',(16.1039039450206,0.52165948705058,4.2093467427251));
#32579=CARTESIAN_POINT('Ctrl Pts',(16.1516197810833,0.106048948556897,4.55200389457816));
#32580=CARTESIAN_POINT('Ctrl Pts',(16.1993356171462,-0.406947971169398,
4.38774737636841));
#32581=CARTESIAN_POINT('Ctrl Pts',(16.247051453209,-0.546238307271431,3.86741647617928));
#32582=CARTESIAN_POINT('Ctrl Pts',(16.2947672892719,-0.183909600849411,
3.46883906597446));
#32583=CARTESIAN_POINT('Ctrl Pts',(16.3424831253347,0.347306121845567,3.55803491444678));
#32584=CARTESIAN_POINT('Ctrl Pts',(16.3901989613975,0.559585288858183,4.05309410148958));
#32585=CARTESIAN_POINT('Ctrl Pts',(16.4379147974604,0.257988674785898,4.49939615817675));
#32586=CARTESIAN_POINT('Ctrl Pts',(16.4856306335232,-0.280522909008289,
4.4870950386126));
#32587=CARTESIAN_POINT('Ctrl Pts',(16.5333464695861,-0.561425989060384,
4.02748705016995));
#32588=CARTESIAN_POINT('Ctrl Pts',(16.5810623056489,-0.326762944709103,
3.54263728061361));
#32589=CARTESIAN_POINT('Ctrl Pts',(16.6287781417117,0.207971539662738,3.4777907336998));
#32590=CARTESIAN_POINT('Ctrl Pts',(16.6764939777746,0.551722559108811,3.89249699125187));
#32591=CARTESIAN_POINT('Ctrl Pts',(16.7242098138374,0.388818263182495,4.40592491588375));
#32592=CARTESIAN_POINT('Ctrl Pts',(16.7719256499003,-0.131143826562283,
4.54658574430191));
#32593=CARTESIAN_POINT('Ctrl Pts',(16.8196414859631,-0.53067452246778,4.18530847342493));
#32594=CARTESIAN_POINT('Ctrl Pts',(16.8673573220259,-0.442878638914007,
3.65385958006445));
#32595=CARTESIAN_POINT('Ctrl Pts',(16.9150731580888,0.0516195133182915,
3.44027676038576));
#32596=CARTESIAN_POINT('Ctrl Pts',(16.9627889941516,0.498714672202087,3.74069640409388));
#32597=CARTESIAN_POINT('Ctrl Pts',(17.0105048302145,0.487832473891125,4.27923852982128));
#32598=CARTESIAN_POINT('Ctrl Pts',(17.0582206662773,0.0289662085384809,
4.56135161697672));
#32599=CARTESIAN_POINT('Ctrl Pts',(17.1059365023401,-0.456500171817451,
4.32796687675757));
#32600=CARTESIAN_POINT('Ctrl Pts',(17.1536523384029,-0.522755420235406,
3.79340510719289));
#32601=CARTESIAN_POINT('Ctrl Pts',(17.2013681744658,-0.108956322625149,
3.44856260656401));
#32602=CARTESIAN_POINT('Ctrl Pts',(17.2490840105286,0.404899042560309,3.61011354928233));
#32603=CARTESIAN_POINT('Ctrl Pts',(17.2967998465915,0.54692938679005,4.12970321886885));
#32604=CARTESIAN_POINT('Ctrl Pts',(17.3445156826543,0.186706059540143,4.53018442682757));
#32605=CARTESIAN_POINT('Ctrl Pts',(17.3922315187172,-0.344972315027459,
4.4437891176945));
#32606=CARTESIAN_POINT('Ctrl Pts',(17.43994735478,-0.559857304624004,3.94985543320929));
#32607=CARTESIAN_POINT('Ctrl Pts',(17.4876631908428,-0.260616716872392,
3.5019702759813));
#32608=CARTESIAN_POINT('Ctrl Pts',(17.5353790269057,0.277952212086773,3.51143347749201));
#32609=CARTESIAN_POINT('Ctrl Pts',(17.5830948629685,0.561273347842132,3.96955483418404));
#32610=CARTESIAN_POINT('Ctrl Pts',(17.6308106990313,0.329168531973526,4.45563445510394));
#32611=CARTESIAN_POINT('Ctrl Pts',(17.6785265350942,-0.205216811715269,
4.52329794506467));
#32612=CARTESIAN_POINT('Ctrl Pts',(17.726242371157,-0.551148399539408,4.11040888009862));
#32613=CARTESIAN_POINT('Ctrl Pts',(17.7739582072198,-0.390951931558304,
3.59612964167903));
#32614=CARTESIAN_POINT('Ctrl Pts',(17.8216740432827,0.128261710741471,3.45273076764982));
#32615=CARTESIAN_POINT('Ctrl Pts',(17.8693898793456,0.529690650507269,3.81189765050732));
#32616=CARTESIAN_POINT('Ctrl Pts',(17.9171057154083,0.44469651557395,4.34380181523062));
#32617=CARTESIAN_POINT('Ctrl Pts',(17.9648215514712,-0.0486692721463468,
4.55998748295674));
#32618=CARTESIAN_POINT('Ctrl Pts',(18.012537387534,-0.497341318381634,4.26192802856871));
#32619=CARTESIAN_POINT('Ctrl Pts',(18.0602532235969,-0.489297179367249,
3.72333603526529));
#32620=CARTESIAN_POINT('Ctrl Pts',(18.1079690596597,-0.0319239117350811,
3.43880881780002));
#32621=CARTESIAN_POINT('Ctrl Pts',(18.1556848957225,0.454765575255941,3.66963209798526));
#32622=CARTESIAN_POINT('Ctrl Pts',(18.2034007317854,0.523836837021606,4.20383730595423));
#32623=CARTESIAN_POINT('Ctrl Pts',(18.2511165678483,0.111860671084556,4.5508555794253));
#32624=CARTESIAN_POINT('Ctrl Pts',(18.298832403911,-0.402838870307115,4.39201469830757));
#32625=CARTESIAN_POINT('Ctrl Pts',(18.346548239974,-0.547605278623001,3.87318068781251));
#32626=CARTESIAN_POINT('Ctrl Pts',(18.3942640760367,-0.189497333589109,
3.47080680306518));
#32627=CARTESIAN_POINT('Ctrl Pts',(18.4419799120997,0.342628928670919,3.55439917374707));
#32628=CARTESIAN_POINT('Ctrl Pts',(18.4896957481624,0.560113773708727,4.04719363962704));
#32629=CARTESIAN_POINT('Ctrl Pts',(18.5374115842253,0.263237521891608,4.49664946007004));
#32630=CARTESIAN_POINT('Ctrl Pts',(18.5851274202881,-0.275373796708506,
4.49002443939646));
#32631=CARTESIAN_POINT('Ctrl Pts',(18.632843256351,-0.561105120620647,4.03340243603));
#32632=CARTESIAN_POINT('Ctrl Pts',(18.6805590924138,-0.331564978554912,
3.54610646169455));
#32633=CARTESIAN_POINT('Ctrl Pts',(18.7282749284766,0.202456385100939,3.47562790763498));
#32634=CARTESIAN_POINT('Ctrl Pts',(18.7759907645394,0.550558935126376,3.8866883144956));
#32635=CARTESIAN_POINT('Ctrl Pts',(18.8237066006023,0.393074743587739,4.40180458567998));
#32636=CARTESIAN_POINT('Ctrl Pts',(18.8714224366651,-0.125376033221007,
4.54793752327491));
#32637=CARTESIAN_POINT('Ctrl Pts',(18.919138272728,-0.528692069562509,4.19089100214638));
#32638=CARTESIAN_POINT('Ctrl Pts',(18.9668541087908,-0.4465020434557,3.6585463365067));
#32639=CARTESIAN_POINT('Ctrl Pts',(19.0145699448537,0.0457176794812401,
3.43976382400136));
#32640=CARTESIAN_POINT('Ctrl Pts',(19.0622857809165,0.495954153879041,3.73545481224116));
#32641=CARTESIAN_POINT('Ctrl Pts',(19.1100016169793,0.490748297561716,4.27408171698104));
#32642=CARTESIAN_POINT('Ctrl Pts',(19.1577174530421,0.0348807284082936,
4.5610151636709));
#32643=CARTESIAN_POINT('Ctrl Pts',(19.205433289105,-0.453018350253257,4.33275975334162));
#32644=CARTESIAN_POINT('Ctrl Pts',(19.2531491251678,-0.524903707479367,
3.79892594114836));
#32645=CARTESIAN_POINT('Ctrl Pts',(19.3008649612307,-0.11476191309534,3.44974153150476));
#32646=CARTESIAN_POINT('Ctrl Pts',(19.3485807972935,0.400767511262006,3.60586793956989));
#32647=CARTESIAN_POINT('Ctrl Pts',(19.3962966333564,0.548265964675035,4.12393188459875));
#32648=CARTESIAN_POINT('Ctrl Pts',(19.4440124694192,0.192283344213529,4.52818727047755));
#32649=CARTESIAN_POINT('Ctrl Pts',(19.491728305482,-0.340276025447905,4.44740016355363));
#32650=CARTESIAN_POINT('Ctrl Pts',(19.5394441415448,-0.560354693525076,
3.95575859308266));
#32651=CARTESIAN_POINT('Ctrl Pts',(19.5871599776077,-0.265851008504119,
3.50474460473346));
#32652=CARTESIAN_POINT('Ctrl Pts',(19.6348758136705,0.272787718306182,3.5085312334714));
#32653=CARTESIAN_POINT('Ctrl Pts',(19.6825916497334,0.560921342594646,3.96364125479661));
#32654=CARTESIAN_POINT('Ctrl Pts',(19.7303074857962,0.33395216026474,4.45213995410186));
#32655=CARTESIAN_POINT('Ctrl Pts',(19.7780233218591,-0.199690227635008,
4.52543179776919));
#32656=CARTESIAN_POINT('Ctrl Pts',(19.8257391579219,-0.549954387748789,
4.11621111891367));
#32657=CARTESIAN_POINT('Ctrl Pts',(19.8734549939848,-0.395186252277308,
3.60027277035845));
#32658=CARTESIAN_POINT('Ctrl Pts',(19.9211708300475,0.122486141425193,3.45140859770427));
#32659=CARTESIAN_POINT('Ctrl Pts',(19.9688866661104,0.527680190865048,3.80632716374734));
#32660=CARTESIAN_POINT('Ctrl Pts',(20.0166025021732,0.448292560087992,4.33909316421112));
#32661=CARTESIAN_POINT('Ctrl Pts',(20.0643183382361,-0.0427598846646947,
4.56047472290141));
#32662=CARTESIAN_POINT('Ctrl Pts',(20.1120341742989,-0.49456253103916,4.26714478353561));
#32663=CARTESIAN_POINT('Ctrl Pts',(20.1597500103618,-0.492168201513856,
3.72852743457374));
#32664=CARTESIAN_POINT('Ctrl Pts',(20.2074658464246,-0.0378697858522375,
3.43914000028616));
#32665=CARTESIAN_POINT('Ctrl Pts',(20.2551816824874,0.451321269441671,3.66492646727415));
#32666=CARTESIAN_POINT('Ctrl Pts',(20.3028975185503,0.52583741886325,4.1981749506787));
#32667=CARTESIAN_POINT('Ctrl Pts',(20.3506133546131,0.117885080656874,4.54989459844945));
#32668=CARTESIAN_POINT('Ctrl Pts',(20.398329190676,-0.399119892637424,4.39574851066478));
#32669=CARTESIAN_POINT('Ctrl Pts',(20.438092387395,-0.523197416260526,3.96600412247733));
#32670=CARTESIAN_POINT('Ctrl Pts',(20.4699029447702,-0.3725623900923,3.67462118354637));
#32671=CARTESIAN_POINT('Ctrl Pts',(20.4937608628016,-0.172533290246804,
3.53519650363565));
#32672=CARTESIAN_POINT('Ctrl Pts',(20.5176187808331,0.0720421502968434,
3.50974356844941));
#32673=CARTESIAN_POINT('Ctrl Pts',(20.5414766988645,0.297725647320748,3.60399556061657));
#32674=CARTESIAN_POINT('Ctrl Pts',(20.5653346168959,0.451286063531533,3.79517586539437));
#32675=CARTESIAN_POINT('Ctrl Pts',(20.5891925349273,0.494134760388362,4.03639109206021));
#32676=CARTESIAN_POINT('Ctrl Pts',(20.6130504529587,0.416344747430809,4.26873428690612));
#32677=CARTESIAN_POINT('Ctrl Pts',(20.6369083709901,0.23664610161733,4.43535054865035));
#32678=CARTESIAN_POINT('Ctrl Pts',(20.6607662890216,-0.000865470816140784,
4.49551919950567));
#32679=CARTESIAN_POINT('Ctrl Pts',(20.684624207053,-0.238193741375527,4.43451595913869));
#32680=CARTESIAN_POINT('Ctrl Pts',(20.7084821250844,-0.417262150572256,
4.26726382233879));
#32681=CARTESIAN_POINT('Ctrl Pts',(20.7323400431158,-0.494306543785295,
4.03465729316116));
#32682=CARTESIAN_POINT('Ctrl Pts',(20.7561979611472,-0.45047531426282,3.79357669839993));
#32683=CARTESIAN_POINT('Ctrl Pts',(20.7800558791787,-0.296492828349621,
3.60297191305088));
#32684=CARTESIAN_POINT('Ctrl Pts',(20.80391379721,-0.0700085893017688,3.50945147432983));
#32685=CARTESIAN_POINT('Ctrl Pts',(20.8277717152415,0.173594031734132,3.53588342526713));
#32686=CARTESIAN_POINT('Ctrl Pts',(20.8516296332729,0.374748514455718,3.6758045671588));
#32687=CARTESIAN_POINT('Ctrl Pts',(20.8754875513043,0.484266602122282,3.89500029884494));
#32688=CARTESIAN_POINT('Ctrl Pts',(20.8993454693358,0.475368407265908,4.13987133054223));
#32689=CARTESIAN_POINT('Ctrl Pts',(20.9232033873671,0.350229638882089,4.35054000504804));
#32690=CARTESIAN_POINT('Ctrl Pts',(20.9470613053986,0.139450209771325,4.47549210343221));
#32691=CARTESIAN_POINT('Ctrl Pts',(20.97091922343,-0.105428607968738,4.48417342845956));
#32692=CARTESIAN_POINT('Ctrl Pts',(20.9947771414615,-0.324527251938122,
4.37446116262749));
#32693=CARTESIAN_POINT('Ctrl Pts',(21.0186350594928,-0.464270146732381,
4.17318294187641));
#32694=CARTESIAN_POINT('Ctrl Pts',(21.0424929775243,-0.490486342136868,
3.92955677471355));
#32695=CARTESIAN_POINT('Ctrl Pts',(21.0663508955557,-0.396765267394252,
3.7031558948169));
#32696=CARTESIAN_POINT('Ctrl Pts',(21.0902088135871,-0.206024276530194,
3.54934148458869));
#32697=CARTESIAN_POINT('Ctrl Pts',(21.1140667316185,0.0350952616297792,
3.50572535702762));
#32698=CARTESIAN_POINT('Ctrl Pts',(21.1379246496499,0.267633052506714,3.58297284346672));
#32699=CARTESIAN_POINT('Ctrl Pts',(21.1617825676814,0.434727271782411,3.76219482925797));
#32700=CARTESIAN_POINT('Ctrl Pts',(21.1856404857128,0.495518831419392,3.99956665698474));
#32701=CARTESIAN_POINT('Ctrl Pts',(21.2094984037442,0.43514253908843,4.23704444887943));
#32702=CARTESIAN_POINT('Ctrl Pts',(21.2333563217756,0.268362042918248,4.41655841606373));
#32703=CARTESIAN_POINT('Ctrl Pts',(21.257214239807,0.0359597172125542,4.49421250369607));
#32704=CARTESIAN_POINT('Ctrl Pts',(21.2810721578384,-0.205235738871087,
4.45101817209691));
#32705=CARTESIAN_POINT('Ctrl Pts',(21.3049300758699,-0.396245466293343,
4.29753761193144));
#32706=CARTESIAN_POINT('Ctrl Pts',(21.3287879939013,-0.490362383696085,
4.07130100088706));
#32707=CARTESIAN_POINT('Ctrl Pts',(21.3526459119327,-0.464572341082516,
3.82762935292545));
#32708=CARTESIAN_POINT('Ctrl Pts',(21.3765038299641,-0.325181706377507,
3.62610702345576));
#32709=CARTESIAN_POINT('Ctrl Pts',(21.4003617479955,-0.106275286691508,
3.51601171139131));
#32710=CARTESIAN_POINT('Ctrl Pts',(21.424219666027,0.138618335471326,3.52426471946798));
#32711=CARTESIAN_POINT('Ctrl Pts',(21.4480775840584,0.349615998723735,3.64884796240357));
#32712=CARTESIAN_POINT('Ctrl Pts',(21.4719355020898,0.475123026939619,3.85929744372095));
#32713=CARTESIAN_POINT('Ctrl Pts',(21.4957934201212,0.484449532977353,4.10415253270923));
#32714=CARTESIAN_POINT('Ctrl Pts',(21.5196513381527,0.375314932061802,4.32353949039209));
#32715=CARTESIAN_POINT('Ctrl Pts',(21.543509256184,0.174405606883644,4.4638122296353));
#32716=CARTESIAN_POINT('Ctrl Pts',(21.5673671742155,-0.069150639890911,
4.49067024474121));
#32717=CARTESIAN_POINT('Ctrl Pts',(21.5912250922469,-0.29579767158652,4.39754601941878));
#32718=CARTESIAN_POINT('Ctrl Pts',(21.6150830102783,-0.450114115212426,
4.20721096341231));
#32719=CARTESIAN_POINT('Ctrl Pts',(21.6389409283097,-0.494365396806572,
3.96620718253823));
#32720=CARTESIAN_POINT('Ctrl Pts',(21.6627988463412,-0.417730872638478,
3.73346666603139));
#32721=CARTESIAN_POINT('Ctrl Pts',(21.6866567643726,-0.238949771349764,
3.56590080990214));
#32722=CARTESIAN_POINT('Ctrl Pts',(21.710514682404,-0.00173894210493873,
3.50448403037633));
#32723=CARTESIAN_POINT('Ctrl Pts',(21.7343726004354,0.235897105852373,3.56423440300754));
#32724=CARTESIAN_POINT('Ctrl Pts',(21.7582305184669,0.415849885720624,3.73054133411992));
#32725=CARTESIAN_POINT('Ctrl Pts',(21.7820884364982,0.49411604100673,3.96273824894669));
#32726=CARTESIAN_POINT('Ctrl Pts',(21.8059463545297,0.451557364815975,4.20404667689569));
#32727=CARTESIAN_POINT('Ctrl Pts',(21.8298042725611,0.29858061275206,4.39546013422383));
#32728=CARTESIAN_POINT('Ctrl Pts',(21.8536621905925,0.0725927676976751,
4.49017281661646));
#32729=CARTESIAN_POINT('Ctrl Pts',(21.8775201086239,-0.171145986446082,
4.46502489330693));
#32730=CARTESIAN_POINT('Ctrl Pts',(21.9013780266554,-0.373034884980705,
4.32616571656009));
#32731=CARTESIAN_POINT('Ctrl Pts',(21.9252359446868,-0.483706592871294,
4.10755013753858));
#32732=CARTESIAN_POINT('Ctrl Pts',(21.9490938627182,-0.476098862901817,
3.86263562028194));
#32733=CARTESIAN_POINT('Ctrl Pts',(21.9729517807496,-0.352071992280181,
3.65131043559696));
#32734=CARTESIAN_POINT('Ctrl Pts',(21.996809698781,-0.141953929297546,3.52524934752154));
#32735=CARTESIAN_POINT('Ctrl Pts',(22.0206676168125,0.102875736145779,3.51527772592526));
#32736=CARTESIAN_POINT('Ctrl Pts',(22.0445255348438,0.322549481822576,3.62383390390986));
#32737=CARTESIAN_POINT('Ctrl Pts',(22.0683834528753,0.46335109312246,3.82437293894729));
#32738=CARTESIAN_POINT('Ctrl Pts',(22.0922413709067,0.490850740723195,4.06785757439707));
#32739=CARTESIAN_POINT('Ctrl Pts',(22.1160992889381,0.398324011712033,4.29474918450382));
#32740=CARTESIAN_POINT('Ctrl Pts',(22.1399572069695,0.208396211707814,4.44956659019228));
#32741=CARTESIAN_POINT('Ctrl Pts',(22.163815125001,-0.0324901386554863,
4.49445271863166));
#32742=CARTESIAN_POINT('Ctrl Pts',(22.1876730430324,-0.265431765108271,
4.41843168874211));
#32743=CARTESIAN_POINT('Ctrl Pts',(22.2115309610638,-0.433468094767725,
4.24009271310828));
#32744=CARTESIAN_POINT('Ctrl Pts',(22.2353888790952,-0.495509667838209,
4.00304452911861));
#32745=CARTESIAN_POINT('Ctrl Pts',(22.2592467971266,-0.436385629680506,
3.76525187484075));
#32746=CARTESIAN_POINT('Ctrl Pts',(22.2831047151581,-0.270553418215538,
3.58486153155103));
#32747=CARTESIAN_POINT('Ctrl Pts',(22.3069626331895,-0.0385635261649252,
3.50598385198694));
#32748=CARTESIAN_POINT('Ctrl Pts',(22.3308205512209,0.202856198284482,3.54790657725669));
#32749=CARTESIAN_POINT('Ctrl Pts',(22.3546784692523,0.394672056935096,3.70037845932536));
#32750=CARTESIAN_POINT('Ctrl Pts',(22.3785363872837,0.489979846308564,3.9261159693126));
#32751=CARTESIAN_POINT('Ctrl Pts',(22.4023943053151,0.465474217808745,4.1699201379362));
#32752=CARTESIAN_POINT('Ctrl Pts',(22.4262522233466,0.327147461276091,4.37217420322137));
#32753=CARTESIAN_POINT('Ctrl Pts',(22.450110141378,0.108824243893236,4.4834215400391));
#32754=CARTESIAN_POINT('Ctrl Pts',(22.4739680594094,-0.136109474402841,
4.47645913832327));
#32755=CARTESIAN_POINT('Ctrl Pts',(22.4978259774408,-0.347760701725541,
4.3529895060813));
#32756=CARTESIAN_POINT('Ctrl Pts',(22.5216838954723,-0.474374996640319,
4.1432043106148));
#32757=CARTESIAN_POINT('Ctrl Pts',(22.5455418135036,-0.484991622785221,
3.89840178635216));
#32758=CARTESIAN_POINT('Ctrl Pts',(22.5693997315351,-0.377014700254462,
3.67844274379546));
#32759=CARTESIAN_POINT('Ctrl Pts',(22.5932576495665,-0.176847198578467,
3.53711330196678));
#32760=CARTESIAN_POINT('Ctrl Pts',(22.6171155675979,0.0665638539184235,
3.50897209184919));
#32761=CARTESIAN_POINT('Ctrl Pts',(22.6409734856293,0.293698998435555,3.60090091054846));
#32762=CARTESIAN_POINT('Ctrl Pts',(22.6648314036608,0.449015288492166,3.79041970485759));
#32763=CARTESIAN_POINT('Ctrl Pts',(22.6886893216922,0.494537845944295,4.03118776656693));
#32764=CARTESIAN_POINT('Ctrl Pts',(22.7125472397236,0.419127261608858,4.26432734830583));
#32765=CARTESIAN_POINT('Ctrl Pts',(22.736405157755,0.241238408088568,4.43283588997321));
#32766=CARTESIAN_POINT('Ctrl Pts',(22.7602630757865,0.00434171083240793,
4.49549632518638));
#32767=CARTESIAN_POINT('Ctrl Pts',(22.7841209938178,-0.233581370990537,
4.43700954435219));
#32768=CARTESIAN_POINT('Ctrl Pts',(22.8079789118493,-0.414457183229959,
4.27163232278894));
#32769=CARTESIAN_POINT('Ctrl Pts',(22.8238841905369,-0.46737397936094,4.11714349286348));
#32770=CARTESIAN_POINT('Ctrl Pts',(22.8318368298807,-0.473742730682552,
4.03823705100924));
#32771=CARTESIAN_POINT('Ctrl Pts',(4.,-0.219892372743211,3.64701365460636));
#32772=CARTESIAN_POINT('Ctrl Pts',(4.00795263934381,-0.161099076858729,
3.61038844940468));
#32773=CARTESIAN_POINT('Ctrl Pts',(4.02385791803142,-0.0249198690254346,
3.56711791692558));
#32774=CARTESIAN_POINT('Ctrl Pts',(4.04771583606284,0.185569069288609,3.60813812632505));
#32775=CARTESIAN_POINT('Ctrl Pts',(4.07157375409426,0.350624105231944,3.74494568050885));
#32776=CARTESIAN_POINT('Ctrl Pts',(4.09543167212568,0.429971014252744,3.94413788601839));
#32777=CARTESIAN_POINT('Ctrl Pts',(4.1192895901571,0.40416308778273,4.15698104289539));
#32778=CARTESIAN_POINT('Ctrl Pts',(4.14314750818851,0.279534313346206,4.3314427366163));
#32779=CARTESIAN_POINT('Ctrl Pts',(4.16700542621994,0.0865475313004802,
4.42485517705098));
#32780=CARTESIAN_POINT('Ctrl Pts',(4.19086334425134,-0.127600227202394,
4.41438026490915));
#32781=CARTESIAN_POINT('Ctrl Pts',(4.21472126228278,-0.310547447266788,
4.30257739619942));
#32782=CARTESIAN_POINT('Ctrl Pts',(4.23857918031418,-0.417556725585918,
4.11678647978038));
#32783=CARTESIAN_POINT('Ctrl Pts',(4.26243709834561,-0.422462345057068,
3.90243789311793));
#32784=CARTESIAN_POINT('Ctrl Pts',(4.28629501637703,-0.324064236326554,
3.71194600226016));
#32785=CARTESIAN_POINT('Ctrl Pts',(4.31015293440845,-0.146423688323203,
3.59189110566319));
#32786=CARTESIAN_POINT('Ctrl Pts',(4.33401085243986,0.0670214896752265,
3.5716299793216));
#32787=CARTESIAN_POINT('Ctrl Pts',(4.35786877047129,0.264078061498623,3.65611697628114));
#32788=CARTESIAN_POINT('Ctrl Pts',(4.38172668850271,0.396560367883193,3.82469274783887));
#32789=CARTESIAN_POINT('Ctrl Pts',(4.40558460653412,0.432072854850341,4.03613591352675));
#32790=CARTESIAN_POINT('Ctrl Pts',(4.42944252456555,0.361931763288092,4.23874286631049));
#32791=CARTESIAN_POINT('Ctrl Pts',(4.45330044259696,0.203288494707987,4.382970683851));
#32792=CARTESIAN_POINT('Ctrl Pts',(4.47715836062838,-0.00506434719902249,
4.43355173791626));
#32793=CARTESIAN_POINT('Ctrl Pts',(4.5010162786598,-0.212178818846594,4.37811758201071));
#32794=CARTESIAN_POINT('Ctrl Pts',(4.52487419669122,-0.367409789343613,
4.23022337776645));
#32795=CARTESIAN_POINT('Ctrl Pts',(4.54873211472264,-0.432799058467291,
4.02603328640456));
#32796=CARTESIAN_POINT('Ctrl Pts',(4.57259003275406,-0.392357168499796,
3.8154773474345));
#32797=CARTESIAN_POINT('Ctrl Pts',(4.59644795078547,-0.255973263285106,
3.65004222328625));
#32798=CARTESIAN_POINT('Ctrl Pts',(4.6203058688169,-0.0569969226013119,
3.57018130821703));
#32799=CARTESIAN_POINT('Ctrl Pts',(4.64416378684831,0.155916718210686,3.59542277130738));
#32800=CARTESIAN_POINT('Ctrl Pts',(4.66802170487973,0.330704474340828,3.71959438727947));
#32801=CARTESIAN_POINT('Ctrl Pts',(4.69187962291115,0.424625978282027,3.91233281365517));
#32802=CARTESIAN_POINT('Ctrl Pts',(4.71573754094257,0.41471486395576,4.1265082550995));
#32803=CARTESIAN_POINT('Ctrl Pts',(4.73959545897399,0.303394668785218,4.30974898215573));
#32804=CARTESIAN_POINT('Ctrl Pts',(4.76345337700541,0.117886212792376,4.41724764568232));
#32805=CARTESIAN_POINT('Ctrl Pts',(4.78731129503683,-0.0964486333844469,
4.42271789424177));
#32806=CARTESIAN_POINT('Ctrl Pts',(4.81116921306824,-0.287199161490599,
4.32482210305491));
#32807=CARTESIAN_POINT('Ctrl Pts',(4.83502713109967,-0.407721671464292,
4.14749845969467));
#32808=CARTESIAN_POINT('Ctrl Pts',(4.85888504913109,-0.42854512664958,3.93410742516172));
#32809=CARTESIAN_POINT('Ctrl Pts',(4.8827429671625,-0.344577625034195,3.73682892005441));
#32810=CARTESIAN_POINT('Ctrl Pts',(4.90660088519393,-0.176351507991885,
3.60390291263011));
#32811=CARTESIAN_POINT('Ctrl Pts',(4.93045880322534,0.0349973564730633,
3.56783343253575));
#32812=CARTESIAN_POINT('Ctrl Pts',(4.95431672125677,0.237788413971502,3.63744045016736));
#32813=CARTESIAN_POINT('Ctrl Pts',(4.97817463928818,0.382433727027559,3.79570315365689));
#32814=CARTESIAN_POINT('Ctrl Pts',(5.0020325573196,0.433563576539811,4.00392200101168));
#32815=CARTESIAN_POINT('Ctrl Pts',(5.02589047535102,0.378675321553375,4.21118181228595));
#32816=CARTESIAN_POINT('Ctrl Pts',(5.04974839338244,0.231190635538481,4.36680191797922));
#32817=CARTESIAN_POINT('Ctrl Pts',(5.07360631141386,0.0271735416279573,
4.43272896324296));
#32818=CARTESIAN_POINT('Ctrl Pts',(5.09746422944527,-0.183488223403015,
4.39284198969348));
#32819=CARTESIAN_POINT('Ctrl Pts',(5.1213221474767,-0.349282119693095,4.256894448863));
#32820=CARTESIAN_POINT('Ctrl Pts',(5.1451800655081,-0.4296670234643,4.05812921762123));
#32821=CARTESIAN_POINT('Ctrl Pts',(5.16903798353954,-0.404986636103755,
3.84514980926298));
#32822=CARTESIAN_POINT('Ctrl Pts',(5.19289590157095,-0.281275984601366,
3.67003549057442));
#32823=CARTESIAN_POINT('Ctrl Pts',(5.21675381960238,-0.0887856930599551,
3.5756064824932));
#32824=CARTESIAN_POINT('Ctrl Pts',(5.24061173763379,0.125415118908336,3.58495324968971));
#32825=CARTESIAN_POINT('Ctrl Pts',(5.26446965566521,0.308948518064291,3.69579025298356));
#32826=CARTESIAN_POINT('Ctrl Pts',(5.28832757369662,0.416935588964862,3.88101482593007));
#32827=CARTESIAN_POINT('Ctrl Pts',(5.31218549172805,0.422970551266107,4.09533451502773));
#32828=CARTESIAN_POINT('Ctrl Pts',(5.33604340975946,0.325577692296299,4.28634231834109));
#32829=CARTESIAN_POINT('Ctrl Pts',(5.35990132779089,0.148572219001774,4.40733162501188));
#32830=CARTESIAN_POINT('Ctrl Pts',(5.3837592458223,-0.0647632088646815,
4.42871725387658));
#32831=CARTESIAN_POINT('Ctrl Pts',(5.40761716385372,-0.26226226804932,4.34526983614494));
#32832=CARTESIAN_POINT('Ctrl Pts',(5.43147508188515,-0.395631058815178,
4.17739453851434));
#32833=CARTESIAN_POINT('Ctrl Pts',(5.45533299991656,-0.432257278927009,
3.96614144408682));
#32834=CARTESIAN_POINT('Ctrl Pts',(5.47919091794798,-0.363184819889405,
3.76316768886851));
#32835=CARTESIAN_POINT('Ctrl Pts',(5.5030488359794,-0.205303779432806,3.61810588490468));
#32836=CARTESIAN_POINT('Ctrl Pts',(5.52690675401082,0.00277962745745752,
3.56642759466814));
#32837=CARTESIAN_POINT('Ctrl Pts',(5.55076467204224,0.210183339719457,3.62076956781107));
#32838=CARTESIAN_POINT('Ctrl Pts',(5.57462259007365,0.36619150013966,3.76784371165257));
#32839=CARTESIAN_POINT('Ctrl Pts',(5.59848050810508,0.432655863921731,3.97168639180759));
#32840=CARTESIAN_POINT('Ctrl Pts',(5.62233842613649,0.393324083661671,4.18245252040861));
#32841=CARTESIAN_POINT('Ctrl Pts',(5.64619634416792,0.257813851021257,4.34860403787086));
#32842=CARTESIAN_POINT('Ctrl Pts',(5.67005426219933,0.0592611090830247,
4.42951237227525));
#32843=CARTESIAN_POINT('Ctrl Pts',(5.69391218023075,-0.153782588238227,
4.40539323200473));
#32844=CARTESIAN_POINT('Ctrl Pts',(5.71777009826218,-0.329222253834466,
4.28214440376531));
#32845=CARTESIAN_POINT('Ctrl Pts',(5.74162801629359,-0.424158110434281,
4.08990358344764));
#32846=CARTESIAN_POINT('Ctrl Pts',(5.76548593432501,-0.415375755386326,
3.8756788878607));
#32847=CARTESIAN_POINT('Ctrl Pts',(5.78934385235642,-0.305022713182347,
3.69185409099321));
#32848=CARTESIAN_POINT('Ctrl Pts',(5.81320177038785,-0.120083309624962,
3.58337936191985));
#32849=CARTESIAN_POINT('Ctrl Pts',(5.83705968841926,0.0942197354074567,
3.57677972866706));
#32850=CARTESIAN_POINT('Ctrl Pts',(5.86091760645069,0.285483486244351,3.673668977605));
#32851=CARTESIAN_POINT('Ctrl Pts',(5.8847755244821,0.406938752801468,3.85035505520226));
#32852=CARTESIAN_POINT('Ctrl Pts',(5.90863344251353,0.428886400972996,4.06363338935351));
#32853=CARTESIAN_POINT('Ctrl Pts',(5.93249136054494,0.345959657594393,4.261351642888));
#32854=CARTESIAN_POINT('Ctrl Pts',(5.95634927857636,0.178436323746589,4.39516226965834));
#32855=CARTESIAN_POINT('Ctrl Pts',(5.98020719660778,-0.0327194942966983,
4.4323450160316));
#32856=CARTESIAN_POINT('Ctrl Pts',(6.0040651146392,-0.23587461323539,4.36380751861078));
#32857=CARTESIAN_POINT('Ctrl Pts',(6.02792303267061,-0.381351759249696,
4.20630938167977));
#32858=CARTESIAN_POINT('Ctrl Pts',(6.05178095070204,-0.433578399193506,
3.9983625870902));
#32859=CARTESIAN_POINT('Ctrl Pts',(6.07563886873346,-0.379782579589031,
3.79081692866841));
#32860=CARTESIAN_POINT('Ctrl Pts',(6.09949678676487,-0.233120953551068,
3.63442082419035));
#32861=CARTESIAN_POINT('Ctrl Pts',(6.12335470479629,-0.0294522997972467,
3.5674214393556));
#32862=CARTESIAN_POINT('Ctrl Pts',(6.14721262282771,0.181413325723775,3.60619428643423));
#32863=CARTESIAN_POINT('Ctrl Pts',(6.17107054085913,0.347927737305898,3.74127281623538));
#32864=CARTESIAN_POINT('Ctrl Pts',(6.19492845889055,0.429346806292137,3.93959933010928));
#32865=CARTESIAN_POINT('Ctrl Pts',(6.21878637692197,0.405811992579865,4.15272917617017));
#32866=CARTESIAN_POINT('Ctrl Pts',(6.24264429495339,0.282982581651336,4.32844890303245));
#32867=CARTESIAN_POINT('Ctrl Pts',(6.26650221298481,0.0910742457207041,
4.42397415233781));
#32868=CARTESIAN_POINT('Ctrl Pts',(6.29036013101623,-0.123327005978964,
4.41559921078967));
#32869=CARTESIAN_POINT('Ctrl Pts',(6.31421804904765,-0.307151379675736,
4.3060270879454));
#32870=CARTESIAN_POINT('Ctrl Pts',(6.33807596707907,-0.416657206472865,
4.12081787696614));
#32871=CARTESIAN_POINT('Ctrl Pts',(6.36193388511048,-0.422829889105799,
3.9075587958503));
#32872=CARTESIAN_POINT('Ctrl Pts',(6.39374444248571,-0.296437506874183,
3.64987069373525));
#32873=CARTESIAN_POINT('Ctrl Pts',(6.43350763920474,0.0703302468340302,
3.51324810367198));
#32874=CARTESIAN_POINT('Ctrl Pts',(6.48122347526758,0.448014600657906,3.7964368525222));
#32875=CARTESIAN_POINT('Ctrl Pts',(6.52893931133042,0.413240052911115,4.26646358767058));
#32876=CARTESIAN_POINT('Ctrl Pts',(6.57665514739325,-0.000480251589724132,
4.49184654025612));
#32877=CARTESIAN_POINT('Ctrl Pts',(6.62437098345609,-0.41404349770976,4.26553045144514));
#32878=CARTESIAN_POINT('Ctrl Pts',(6.67208681951894,-0.447234019333667,
3.79538894860702));
#32879=CARTESIAN_POINT('Ctrl Pts',(6.71980265558177,-0.0698021891909718,
3.51313682319347));
#32880=CARTESIAN_POINT('Ctrl Pts',(6.76751849164461,0.371772181936036,3.67798293440124));
#32881=CARTESIAN_POINT('Ctrl Pts',(6.81523432770745,0.471920133146607,4.13853999974893));
#32882=CARTESIAN_POINT('Ctrl Pts',(6.86295016377028,0.138708377331583,4.4718748549198));
#32883=CARTESIAN_POINT('Ctrl Pts',(6.91066599983312,-0.32188767172048,4.37187913281409));
#32884=CARTESIAN_POINT('Ctrl Pts',(6.95838183589596,-0.486886005735063,
3.93038141845316));
#32885=CARTESIAN_POINT('Ctrl Pts',(7.0060976719588,-0.204771183672361,3.55281534000283));
#32886=CARTESIAN_POINT('Ctrl Pts',(7.05381350802163,0.265389096458903,3.58590591031157));
#32887=CARTESIAN_POINT('Ctrl Pts',(7.10152934408448,0.491837993618785,3.99926540470374));
#32888=CARTESIAN_POINT('Ctrl Pts',(7.14924518014731,0.266624753986561,4.41329951581085));
#32889=CARTESIAN_POINT('Ctrl Pts',(7.19696101621015,-0.203434237821079,
4.44779430805676));
#32890=CARTESIAN_POINT('Ctrl Pts',(7.24467685227299,-0.486676365692783,
4.07107270446015));
#32891=CARTESIAN_POINT('Ctrl Pts',(7.29239268833582,-0.322996137187983,
3.62908393881966));
#32892=CARTESIAN_POINT('Ctrl Pts',(7.34010852439867,0.137296434535941,3.52771310152703));
#32893=CARTESIAN_POINT('Ctrl Pts',(7.3878243604615,0.471507566988788,3.86005058906394));
#32894=CARTESIAN_POINT('Ctrl Pts',(7.43554019652434,0.372726051350611,4.32090577464778));
#32895=CARTESIAN_POINT('Ctrl Pts',(7.48325603258718,-0.0683355354161961,
4.48706824929225));
#32896=CARTESIAN_POINT('Ctrl Pts',(7.53097186865002,-0.44664354691983,4.20594845626764));
#32897=CARTESIAN_POINT('Ctrl Pts',(7.57868770471286,-0.414791917646955,
3.73570302684109));
#32898=CARTESIAN_POINT('Ctrl Pts',(7.62640354077569,-0.00203048755240202,
3.50816557464413));
#32899=CARTESIAN_POINT('Ctrl Pts',(7.67411937683853,0.412595570264971,3.73228724307244));
#32900=CARTESIAN_POINT('Ctrl Pts',(7.72183521290137,0.448328767436039,4.20225365549051));
#32901=CARTESIAN_POINT('Ctrl Pts',(7.7695510489642,0.0723547589785895,4.48648742399228));
#32902=CARTESIAN_POINT('Ctrl Pts',(7.81726688502705,-0.370063737934377,
4.32397230547438));
#32903=CARTESIAN_POINT('Ctrl Pts',(7.86498272108989,-0.472647010158531,
3.86394843388276));
#32904=CARTESIAN_POINT('Ctrl Pts',(7.91269855715272,-0.141191260335066,
3.52886280888004));
#32905=CARTESIAN_POINT('Ctrl Pts',(7.96041439321556,0.31992259635559,3.62642971585976));
#32906=CARTESIAN_POINT('Ctrl Pts',(8.0081302292784,0.48724661017382,4.0670519628834));
#32907=CARTESIAN_POINT('Ctrl Pts',(8.05584606534124,0.207124564615173,4.44609936066402));
#32908=CARTESIAN_POINT('Ctrl Pts',(8.10356190140407,-0.263203155649882,
4.41548685142597));
#32909=CARTESIAN_POINT('Ctrl Pts',(8.15127773746691,-0.491827368180951,
4.00332637343646));
#32910=CARTESIAN_POINT('Ctrl Pts',(8.19899357352975,-0.268798940774433,
3.58811123553743));
#32911=CARTESIAN_POINT('Ctrl Pts',(8.24670940959259,0.201071689948468,3.55113988776764));
#32912=CARTESIAN_POINT('Ctrl Pts',(8.29442524565542,0.486295093906121,3.92636368766143));
#32913=CARTESIAN_POINT('Ctrl Pts',(8.34214108171827,0.324946230517931,4.36920884621601));
#32914=CARTESIAN_POINT('Ctrl Pts',(8.3898569177811,-0.134805756295296,4.47300384028212));
#32915=CARTESIAN_POINT('Ctrl Pts',(8.43757275384394,-0.470763542849379,
4.14243212971755));
#32916=CARTESIAN_POINT('Ctrl Pts',(8.48528858990678,-0.37441192437669,3.68106280283335));
#32917=CARTESIAN_POINT('Ctrl Pts',(8.53300442596962,0.0657679253190804,
3.51257841158684));
#32918=CARTESIAN_POINT('Ctrl Pts',(8.58072026203246,0.445552077224736,3.79170076492532));
#32919=CARTESIAN_POINT('Ctrl Pts',(8.62843609809529,0.41617890091499,4.26210751092856));
#32920=CARTESIAN_POINT('Ctrl Pts',(8.67615193415813,0.0046222361594965,
4.49181689660367));
#32921=CARTESIAN_POINT('Ctrl Pts',(8.72386777022097,-0.411179099183508,
4.26988325855195));
#32922=CARTESIAN_POINT('Ctrl Pts',(8.7715836062838,-0.449388340942622,3.80011167148426));
#32923=CARTESIAN_POINT('Ctrl Pts',(8.81929944234665,-0.0749173544856965,
3.51390061216986));
#32924=CARTESIAN_POINT('Ctrl Pts',(8.86701527840948,0.368351391347115,3.67408210030036));
#32925=CARTESIAN_POINT('Ctrl Pts',(8.91473111447233,0.473357386691186,4.13355901061654));
#32926=CARTESIAN_POINT('Ctrl Pts',(8.96244695053515,0.14367201029714,4.47038662641401));
#32927=CARTESIAN_POINT('Ctrl Pts',(9.01016278659801,-0.317949583830803,
4.37525096534692));
#32928=CARTESIAN_POINT('Ctrl Pts',(9.05787862266083,-0.487593182843731,
3.93551656882348));
#32929=CARTESIAN_POINT('Ctrl Pts',(9.10559445872368,-0.209472459465777,
3.55499829935456));
#32930=CARTESIAN_POINT('Ctrl Pts',(9.15331029478651,0.261010046587687,3.58313193881964));
#32931=CARTESIAN_POINT('Ctrl Pts',(9.20102613084934,0.491803010703882,3.99408193320625));
#32932=CARTESIAN_POINT('Ctrl Pts',(9.2487419669122,0.270965702728691,4.41046657939073));
#32933=CARTESIAN_POINT('Ctrl Pts',(9.29645780297501,-0.198703579405513,
4.44991344988054));
#32934=CARTESIAN_POINT('Ctrl Pts',(9.34417363903789,-0.485900307124067,
4.07619787653679));
#32935=CARTESIAN_POINT('Ctrl Pts',(9.39188947510068,-0.326887306273347,
3.63250862071426));
#32936=CARTESIAN_POINT('Ctrl Pts',(9.43960531116356,0.13231133773591,3.52629235307153));
#32937=CARTESIAN_POINT('Ctrl Pts',(9.48732114722637,0.470006444430667,3.85508910653225));
#32938=CARTESIAN_POINT('Ctrl Pts',(9.53503698328922,0.376087401226012,4.31695976320512));
#32939=CARTESIAN_POINT('Ctrl Pts',(9.58275281935206,-0.0631984893729827,
4.48776139227388));
#32940=CARTESIAN_POINT('Ctrl Pts',(9.63046865541489,-0.444448234747017,
4.21064422964382));
#32941=CARTESIAN_POINT('Ctrl Pts',(9.67818449147773,-0.41755432743774,3.74008922975375));
#32942=CARTESIAN_POINT('Ctrl Pts',(9.72590032754057,-0.00721385634321597,
3.50821428942208));
#32943=CARTESIAN_POINT('Ctrl Pts',(9.77361616360341,0.40975121003073,3.72795373420991));
#32944=CARTESIAN_POINT('Ctrl Pts',(9.82133199966624,0.450435435400681,4.19751745084266));
#32945=CARTESIAN_POINT('Ctrl Pts',(9.86904783572909,0.077477869602138,4.48569785316993));
#32946=CARTESIAN_POINT('Ctrl Pts',(9.91676367179192,-0.366628816002305,
4.3278544435092));
#32947=CARTESIAN_POINT('Ctrl Pts',(9.96447950785476,-0.474054618562381,
3.8689372536849));
#32948=CARTESIAN_POINT('Ctrl Pts',(10.0121953439176,-0.146148770628728,
3.53037700046135));
#32949=CARTESIAN_POINT('Ctrl Pts',(10.0599111799804,0.315967742161179,3.62307877379278));
#32950=CARTESIAN_POINT('Ctrl Pts',(10.1076270160433,0.487926215535836,4.06191310882887));
#32951=CARTESIAN_POINT('Ctrl Pts',(10.1553428521061,0.211814537474087,4.44389168337175));
#32952=CARTESIAN_POINT('Ctrl Pts',(10.203058688169,-0.258809689535701,4.4182376949229));
#32953=CARTESIAN_POINT('Ctrl Pts',(10.2507745242318,-0.491764996345908,
4.00850959581219));
#32954=CARTESIAN_POINT('Ctrl Pts',(10.2984903602946,-0.273124940234581,
3.59096700393021));
#32955=CARTESIAN_POINT('Ctrl Pts',(10.3462061963575,0.196329951061554,3.54904570612073));
#32956=CARTESIAN_POINT('Ctrl Pts',(10.3939220324203,0.485492027373267,3.92124267520431));
#32957=CARTESIAN_POINT('Ctrl Pts',(10.4416378684831,0.328819304693055,4.36576370748498));
#32958=CARTESIAN_POINT('Ctrl Pts',(10.489353704546,-0.129813245022134,4.47439829918413));
#32959=CARTESIAN_POINT('Ctrl Pts',(10.5370695406088,-0.469236294399976,
4.14738563318641));
#32960=CARTESIAN_POINT('Ctrl Pts',(10.5847853766716,-0.377752434501872,
3.68502647241413));
#32961=CARTESIAN_POINT('Ctrl Pts',(10.6325012127345,0.0606272984676223,
3.51191234851464));
#32962=CARTESIAN_POINT('Ctrl Pts',(10.6802170487973,0.443332050383407,3.78701662516801));
#32963=CARTESIAN_POINT('Ctrl Pts',(10.7279328848602,0.418918158891686,4.25770681210006));
#32964=CARTESIAN_POINT('Ctrl Pts',(10.775648720923,0.00980527620531799,
4.49174086815163));
#32965=CARTESIAN_POINT('Ctrl Pts',(10.8233645569858,-0.408311942493964,
4.27420171857372));
#32966=CARTESIAN_POINT('Ctrl Pts',(10.8710803930487,-0.451470021714238,
3.80485891169382));
#32967=CARTESIAN_POINT('Ctrl Pts',(10.9187962291115,-0.080036233235122,
3.51471716883706));
#32968=CARTESIAN_POINT('Ctrl Pts',(10.9665120651743,0.364896059739551,3.6702181168734));
#32969=CARTESIAN_POINT('Ctrl Pts',(11.0142279012372,0.47473868640782,4.1285628425314));
#32970=CARTESIAN_POINT('Ctrl Pts',(11.0619437373,0.148621472554162,4.46884633169921));
#32971=CARTESIAN_POINT('Ctrl Pts',(11.1096595733629,-0.313977126381285,
4.37858102033954));
#32972=CARTESIAN_POINT('Ctrl Pts',(11.1573754094257,-0.488245699001722,
3.94065893278431));
#32973=CARTESIAN_POINT('Ctrl Pts',(11.2050912454886,-0.214150733603143,
3.55723066033293));
#32974=CARTESIAN_POINT('Ctrl Pts',(11.2528070815514,0.256602145595791,3.58040428537983));
#32975=CARTESIAN_POINT('Ctrl Pts',(11.3005229176142,0.491713326162588,3.98889911147238));
#32976=CARTESIAN_POINT('Ctrl Pts',(11.3482387536771,0.275276593332242,4.40758805430897));
#32977=CARTESIAN_POINT('Ctrl Pts',(11.3959545897399,-0.193950870829933,
4.45198261532529));
#32978=CARTESIAN_POINT('Ctrl Pts',(11.4436704258028,-0.485070265991237,
4.08131458604192));
#32979=CARTESIAN_POINT('Ctrl Pts',(11.4913862618656,-0.330742172127369,
3.63597412121053));
#32980=CARTESIAN_POINT('Ctrl Pts',(11.5391020979284,0.127311547523522,3.52492422212962));
#32981=CARTESIAN_POINT('Ctrl Pts',(11.5868179339912,0.468453114143607,3.85014371984754));
#32982=CARTESIAN_POINT('Ctrl Pts',(11.6345337700541,0.379406977967949,4.31297854546471));
#32983=CARTESIAN_POINT('Ctrl Pts',(11.6822496061169,-0.0580544240024287,
4.48840035698771));
#32984=CARTESIAN_POINT('Ctrl Pts',(11.7299654421798,-0.44220355512924,4.21531660568344));
#32985=CARTESIAN_POINT('Ctrl Pts',(11.7776812782426,-0.420270357404582,
3.74450430230823));
#32986=CARTESIAN_POINT('Ctrl Pts',(11.8253971143054,-0.0123964237846327,
3.50831762943));
#32987=CARTESIAN_POINT('Ctrl Pts',(11.8731129503683,0.406861336540243,3.72365044295193));
#32988=CARTESIAN_POINT('Ctrl Pts',(11.9208287864311,0.452492071153857,4.1927593068956));
#32989=CARTESIAN_POINT('Ctrl Pts',(11.968544622494,0.0825923743414284,4.48485433333386));
#32990=CARTESIAN_POINT('Ctrl Pts',(12.0162604585568,-0.363153170675764,
4.33170016502878));
#32991=CARTESIAN_POINT('Ctrl Pts',(12.0639762946196,-0.475409571231627,
3.87394063131468));
#32992=CARTESIAN_POINT('Ctrl Pts',(12.1116921306825,-0.151090047408964,
3.53194335553704));
#32993=CARTESIAN_POINT('Ctrl Pts',(12.1594079667453,0.311977791768556,3.61976969834691));
#32994=CARTESIAN_POINT('Ctrl Pts',(12.2071238028081,0.488551624369653,4.05676737776005));
#32995=CARTESIAN_POINT('Ctrl Pts',(12.254839638871,0.216480982979095,4.44163470069774));
#32996=CARTESIAN_POINT('Ctrl Pts',(12.3025554749338,-0.254387476069249,
4.42094208256136));
#32997=CARTESIAN_POINT('Ctrl Pts',(12.3502713109967,-0.49164800158875,4.0136918729824));
#32998=CARTESIAN_POINT('Ctrl Pts',(12.3979871470595,-0.277420602272412,
3.59386820576715));
#32999=CARTESIAN_POINT('Ctrl Pts',(12.4457029831224,0.191566404775332,3.54700161433684));
#33000=CARTESIAN_POINT('Ctrl Pts',(12.4934188191852,0.484635034689867,3.91613041073711));
#33001=CARTESIAN_POINT('Ctrl Pts',(12.541134655248,0.332655855180181,4.362277941457));
#33002=CARTESIAN_POINT('Ctrl Pts',(12.5888504913109,-0.124806314709729,
4.47574006417428));
#33003=CARTESIAN_POINT('Ctrl Pts',(12.6365663273737,-0.4676569254097,4.15232276575852));
#33004=CARTESIAN_POINT('Ctrl Pts',(12.6842821634365,-0.381050985679211,
3.68902512775968));
#33005=CARTESIAN_POINT('Ctrl Pts',(12.7319979994994,0.0554799374235607,
3.5113004999026));
#33006=CARTESIAN_POINT('Ctrl Pts',(12.7797138355622,0.441062780321708,3.78235614259331));
#33007=CARTESIAN_POINT('Ctrl Pts',(12.8274296716251,0.421610885427219,4.2532774884218));
#33008=CARTESIAN_POINT('Ctrl Pts',(12.8751455076879,0.0149872271275763,
4.49161021945745));
#33009=CARTESIAN_POINT('Ctrl Pts',(12.9228613437507,-0.405399432451448,
4.27848972156979));
#33010=CARTESIAN_POINT('Ctrl Pts',(12.9705771798136,-0.453501555338242,
3.80962782724943));
#33011=CARTESIAN_POINT('Ctrl Pts',(13.0182930158764,-0.0851462219395619,
3.51558762841831));
#33012=CARTESIAN_POINT('Ctrl Pts',(13.0660088519392,0.361400197209248,3.66639076405307));
#33013=CARTESIAN_POINT('Ctrl Pts',(13.1137246880021,0.476067254403989,4.1235523942958));
#33014=CARTESIAN_POINT('Ctrl Pts',(13.1614405240649,0.153554426643267,4.46725395975876));
#33015=CARTESIAN_POINT('Ctrl Pts',(13.2091563601278,-0.30996979384252,4.38186902434892));
#33016=CARTESIAN_POINT('Ctrl Pts',(13.2568721961906,-0.488843983144383,
3.94580788806928));
#33017=CARTESIAN_POINT('Ctrl Pts',(13.3045880322534,-0.218805220893238,
3.55951220202843));
#33018=CARTESIAN_POINT('Ctrl Pts',(13.3523038683163,0.252165742455243,3.57772323864086));
#33019=CARTESIAN_POINT('Ctrl Pts',(13.4000197043791,0.491569024438394,3.98371752277252));
#33020=CARTESIAN_POINT('Ctrl Pts',(13.447735540442,0.279556907518101,4.40466425628032));
#33021=CARTESIAN_POINT('Ctrl Pts',(13.4954513765048,-0.189176619112,4.45400157668594));
#33022=CARTESIAN_POINT('Ctrl Pts',(13.5431672125676,-0.484186345555107,
4.08642226350871));
#33023=CARTESIAN_POINT('Ctrl Pts',(13.5908830486304,-0.334560300710407,
3.63948005597396));
#33024=CARTESIAN_POINT('Ctrl Pts',(13.6385988846933,0.122297616148583,3.52360886035071));
#33025=CARTESIAN_POINT('Ctrl Pts',(13.6863147207561,0.466847750307624,3.8452149784873));
#33026=CARTESIAN_POINT('Ctrl Pts',(13.734030556819,0.3826844119832,4.30896256355269));
#33027=CARTESIAN_POINT('Ctrl Pts',(13.7817463928818,-0.0529039102219543,
4.48898507250754));
#33028=CARTESIAN_POINT('Ctrl Pts',(13.8294622289446,-0.439909757638992,
4.21996506537626));
#33029=CARTESIAN_POINT('Ctrl Pts',(13.8771780650075,-0.422939705734467,
3.74894775411238));
#33030=CARTESIAN_POINT('Ctrl Pts',(13.9248939010703,-0.0175776142901187,
3.50847558318244));
#33031=CARTESIAN_POINT('Ctrl Pts',(13.9726097371332,0.403926270823208,3.71937784729135));
#33032=CARTESIAN_POINT('Ctrl Pts',(14.020325573196,0.454498446235019,4.18797975215946));
#33033=CARTESIAN_POINT('Ctrl Pts',(14.0680414092588,0.0876977051117048,
4.48395695817926));
#33034=CARTESIAN_POINT('Ctrl Pts',(14.1157572453217,-0.359637188018331,
4.33550904286807));
#33035=CARTESIAN_POINT('Ctrl Pts',(14.1634730813845,-0.476711717661702,
3.87895801102093));
#33036=CARTESIAN_POINT('Ctrl Pts',(14.2111889174473,-0.156014541823709,
3.53356170012368));
#33037=CARTESIAN_POINT('Ctrl Pts',(14.2589047535102,0.307953188363286,3.61650285707861));
#33038=CARTESIAN_POINT('Ctrl Pts',(14.306620589573,0.4891227672074,4.05161534124029));
#33039=CARTESIAN_POINT('Ctrl Pts',(14.3543364256359,0.2211233828038,4.4393286633369));
#33040=CARTESIAN_POINT('Ctrl Pts',(14.4020522616987,-0.249937006449114,
4.42359971395084));
#33041=CARTESIAN_POINT('Ctrl Pts',(14.4497680977616,-0.491476396904638,
4.01887262932433));
#33042=CARTESIAN_POINT('Ctrl Pts',(14.4974839338244,-0.281685449746218,
3.59681451879656));
#33043=CARTESIAN_POINT('Ctrl Pts',(14.5451997698872,0.186781580201919,3.54500783946397));
#33044=CARTESIAN_POINT('Ctrl Pts',(14.59291560595,0.483724211046603,3.91102746210588));
#33045=CARTESIAN_POINT('Ctrl Pts',(14.6406314420129,0.33645545583349,4.35875193531444));
#33046=CARTESIAN_POINT('Ctrl Pts',(14.6883472780757,-0.119785521504147,
4.47702898621568));
#33047=CARTESIAN_POINT('Ctrl Pts',(14.7360631141386,-0.466025611307368,
4.15724297904063));
#33048=CARTESIAN_POINT('Ctrl Pts',(14.7837789502014,-0.38430721152129,3.69305832471834));
#33049=CARTESIAN_POINT('Ctrl Pts',(14.8314947862642,0.0503264139313189,
3.51074293371195));
#33050=CARTESIAN_POINT('Ctrl Pts',(14.8792106223271,0.438744519099385,3.77771983486548));
#33051=CARTESIAN_POINT('Ctrl Pts',(14.9269264583899,0.42425678142631,4.24882003188202));
#33052=CARTESIAN_POINT('Ctrl Pts',(14.9746422944528,0.0201675133397715,
4.49142496503298));
#33053=CARTESIAN_POINT('Ctrl Pts',(15.0223581305156,-0.402441892563756,
4.28274679124913));
#33054=CARTESIAN_POINT('Ctrl Pts',(15.0700739665785,-0.455482716161518,
3.8144178884426));
#33055=CARTESIAN_POINT('Ctrl Pts',(15.1177898026413,-0.0902467530057116,
3.51651189422706));
#33056=CARTESIAN_POINT('Ctrl Pts',(15.1655056387041,0.357864192060027,3.66260046696357));
#33057=CARTESIAN_POINT('Ctrl Pts',(15.2132214747669,0.47734294310866,4.11852822244656));
#33058=CARTESIAN_POINT('Ctrl Pts',(15.2609373108298,0.15847032463534,4.46560968746574));
#33059=CARTESIAN_POINT('Ctrl Pts',(15.3086531468926,-0.305928031329979,
4.38511461215921));
#33060=CARTESIAN_POINT('Ctrl Pts',(15.3563689829555,-0.489387968817152,
3.95096286275689));
#33061=CARTESIAN_POINT('Ctrl Pts',(15.4040848190183,-0.223435404337718,
3.56184267101825));
#33062=CARTESIAN_POINT('Ctrl Pts',(15.4518006550811,0.24770132994065,3.57508909640066));
#33063=CARTESIAN_POINT('Ctrl Pts',(15.499516491144,0.491370121559653,3.97853774265298));
#33064=CARTESIAN_POINT('Ctrl Pts',(15.5472323272068,0.283806169849271,4.40169551006635));
#33065=CARTESIAN_POINT('Ctrl Pts',(15.5949481632697,-0.184381354552937,
4.4559701097059));
#33066=CARTESIAN_POINT('Ctrl Pts',(15.6426639993325,-0.483248643997369,
4.09152034160055));
#33067=CARTESIAN_POINT('Ctrl Pts',(15.6903798353953,-0.338341267922855,
3.64302603558196));
#33068=CARTESIAN_POINT('Ctrl Pts',(15.7380956714582,0.117270100534806,3.52234641383892));
#33069=CARTESIAN_POINT('Ctrl Pts',(15.785811507521,0.465190531238913,3.84030342991275));
#33070=CARTESIAN_POINT('Ctrl Pts',(15.8335273435838,0.385919339229949,4.30491226354526));
#33071=CARTESIAN_POINT('Ctrl Pts',(15.8812431796467,-0.0477475201261761,
4.48951547388594));
#33072=CARTESIAN_POINT('Ctrl Pts',(15.9289590157095,-0.437567097060412,
4.22458909239344));
#33073=CARTESIAN_POINT('Ctrl Pts',(15.9766748517724,-0.425562075928853,
3.75341909160864));
#33074=CARTESIAN_POINT('Ctrl Pts',(16.0243906878352,-0.0227568523576073,
3.50868813313462));
#33075=CARTESIAN_POINT('Ctrl Pts',(16.072106523898,0.400946338892803,3.71513642180785));
#33076=CARTESIAN_POINT('Ctrl Pts',(16.1198223599609,0.456454337785543,4.1831793175245));
#33077=CARTESIAN_POINT('Ctrl Pts',(16.1675381960237,0.0927932948370443,
4.4830058273823));
#33078=CARTESIAN_POINT('Ctrl Pts',(16.2152540320865,-0.356081258568678,
4.33928065395499));
#33079=CARTESIAN_POINT('Ctrl Pts',(16.2629698681494,-0.477960913216358,
3.88398883549692));
#33080=CARTESIAN_POINT('Ctrl Pts',(16.3106857042122,-0.160921706883503,
3.53523185446324));
#33081=CARTESIAN_POINT('Ctrl Pts',(16.358401540275,0.303894378979202,3.6132786128531));
#33082=CARTESIAN_POINT('Ctrl Pts',(16.4061173763379,0.489639580609251,4.04645757153336));
#33083=CARTESIAN_POINT('Ctrl Pts',(16.4538332124007,0.225741221292456,4.43697382743292));
#33084=CARTESIAN_POINT('Ctrl Pts',(16.5015490484636,-0.245458775012363,
4.42621029389423));
#33085=CARTESIAN_POINT('Ctrl Pts',(16.5492648845264,-0.4912502013546,4.02405128938415));
#33086=CARTESIAN_POINT('Ctrl Pts',(16.5969807205893,-0.285919008936969,
3.59980561575594));
#33087=CARTESIAN_POINT('Ctrl Pts',(16.6446965566521,0.181976008816936,3.54306460296116));
#33088=CARTESIAN_POINT('Ctrl Pts',(16.6924123927149,0.482759657613431,3.90593439612197));
#33089=CARTESIAN_POINT('Ctrl Pts',(16.7401282287778,0.340217684611379,4.35518608070932));
#33090=CARTESIAN_POINT('Ctrl Pts',(16.7878440648406,-0.114751423091257,
4.47826492214097));
#33091=CARTESIAN_POINT('Ctrl Pts',(16.8355599009034,-0.464342533291602,
4.16214572651883));
#33092=CARTESIAN_POINT('Ctrl Pts',(16.8832757369663,-0.387520750342007,
3.69712561530174));
#33093=CARTESIAN_POINT('Ctrl Pts',(16.9309915730291,0.0451673004198413,
3.51023971187451));
#33094=CARTESIAN_POINT('Ctrl Pts',(16.978707409092,0.436377524217892,3.7731082169636));
#33095=CARTESIAN_POINT('Ctrl Pts',(17.0264232451548,0.426855552995382,4.24433493759383));
#33096=CARTESIAN_POINT('Ctrl Pts',(17.0741390812176,0.0253455594402812,
4.49118512545541));
#33097=CARTESIAN_POINT('Ctrl Pts',(17.1218549172805,-0.399439651340385,
4.28697245475663));
#33098=CARTESIAN_POINT('Ctrl Pts',(17.1695707533433,-0.457413284126125,
3.81922856321607));
#33099=CARTESIAN_POINT('Ctrl Pts',(17.2172865894061,-0.0953372598908034,
3.51748986360026));
#33100=CARTESIAN_POINT('Ctrl Pts',(17.265002425469,0.354288437054553,3.6588476466131));
#33101=CARTESIAN_POINT('Ctrl Pts',(17.3127182615318,0.478565610824392,4.11349088504481));
#33102=CARTESIAN_POINT('Ctrl Pts',(17.3604340975947,0.163368620495752,4.46391369745815));
#33103=CARTESIAN_POINT('Ctrl Pts',(17.4081499336575,-0.301852287783465,
4.38831742326589));
#33104=CARTESIAN_POINT('Ctrl Pts',(17.4558657697204,-0.489877595596684,
3.956123284257));
#33105=CARTESIAN_POINT('Ctrl Pts',(17.5035816057832,-0.228040769637767,
3.56422180844494));
#33106=CARTESIAN_POINT('Ctrl Pts',(17.551297441846,0.243209403937772,3.57250215124727));
#33107=CARTESIAN_POINT('Ctrl Pts',(17.5990132779089,0.491116639619549,3.97336034645914));
#33108=CARTESIAN_POINT('Ctrl Pts',(17.6467291139717,0.288023908337871,4.39868214542132));
#33109=CARTESIAN_POINT('Ctrl Pts',(17.6944449500345,-0.179565609787963,
4.45788799572981));
#33110=CARTESIAN_POINT('Ctrl Pts',(17.7421607860973,-0.48225726547346,4.09660825404716));
#33111=CARTESIAN_POINT('Ctrl Pts',(17.7898766221602,-0.342084653792828,
3.64661166616396));
#33112=CARTESIAN_POINT('Ctrl Pts',(17.837592458223,0.112229559114723,3.52113702282083));
#33113=CARTESIAN_POINT('Ctrl Pts',(17.8853082942859,0.463481641013499,3.83540961967535));
#33114=CARTESIAN_POINT('Ctrl Pts',(17.9330241303487,0.389111400387848,4.30082809533052));
#33115=CARTESIAN_POINT('Ctrl Pts',(17.9807399664116,-0.0425858264624495,
4.48999150220845));
#33116=CARTESIAN_POINT('Ctrl Pts',(18.0284558024744,-0.435175833605105,
4.22918817311999));
#33117=CARTESIAN_POINT('Ctrl Pts',(18.0761716385373,-0.428137176707308,
3.75791781814212));
#33118=CARTESIAN_POINT('Ctrl Pts',(18.1238874746,-0.0279335627019553,3.5089552556775));
#33119=CARTESIAN_POINT('Ctrl Pts',(18.1716033106629,0.397921871745719,3.71092663761881));
#33120=CARTESIAN_POINT('Ctrl Pts',(18.2193191467257,0.458359528554279,4.17835853620019));
#33121=CARTESIAN_POINT('Ctrl Pts',(18.2670349827886,0.097878577523561,4.48200104659009));
#33122=CARTESIAN_POINT('Ctrl Pts',(18.3147508188514,-0.352485777302551,
4.34301457935691));
#33123=CARTESIAN_POINT('Ctrl Pts',(18.3624666549143,-0.479157019140895,
3.88903254594255));
#33124=CARTESIAN_POINT('Ctrl Pts',(18.4101824909771,-0.165810997523729,
3.5369536330429));
#33125=CARTESIAN_POINT('Ctrl Pts',(18.4578983270399,0.299801814449608,3.61009732380414));
#33126=CARTESIAN_POINT('Ctrl Pts',(18.5056141631028,0.49010200717001,4.04129464153984));
#33127=CARTESIAN_POINT('Ctrl Pts',(18.5533299991656,0.230333985517487,4.43457045454981));
#33128=CARTESIAN_POINT('Ctrl Pts',(18.6010458352284,-0.24095327917969,4.42877353242069));
#33129=CARTESIAN_POINT('Ctrl Pts',(18.6487616712913,-0.49096944006335,4.0292272779409));
#33130=CARTESIAN_POINT('Ctrl Pts',(18.6964775073541,-0.290120809601049,
3.60284116440841));
#33131=CARTESIAN_POINT('Ctrl Pts',(18.744193343417,0.177150224400508,3.54117212067402));
#33132=CARTESIAN_POINT('Ctrl Pts',(18.7919091794797,0.481741481528227,3.90085177849878));
#33133=CARTESIAN_POINT('Ctrl Pts',(18.8396250155427,0.343942123623612,4.35158077372017));
#33134=CARTESIAN_POINT('Ctrl Pts',(18.8873408516054,-0.109704578635382,
4.47944773466767));
#33135=CARTESIAN_POINT('Ctrl Pts',(18.9350566876684,-0.462607878309702,
4.16703046362027));
#33136=CARTESIAN_POINT('Ctrl Pts',(18.9827725237311,-0.39069124519864,3.70122654773242));
#33137=CARTESIAN_POINT('Ctrl Pts',(19.030488359794,0.0400031699426168,3.50979089028978));
#33138=CARTESIAN_POINT('Ctrl Pts',(19.0782041958568,0.433962058584907,3.76852180111673));
#33139=CARTESIAN_POINT('Ctrl Pts',(19.1259200319197,0.429406911488226,4.23982270375453));
#33140=CARTESIAN_POINT('Ctrl Pts',(19.1736358679825,0.0305207902517796,
4.49089072733801));
#33141=CARTESIAN_POINT('Ctrl Pts',(19.2213517040454,-0.396393042209671,
4.29116624277653));
#33142=CARTESIAN_POINT('Ctrl Pts',(19.2690675401082,-0.459293044881286,
3.82405931712685));
#33143=CARTESIAN_POINT('Ctrl Pts',(19.316783376171,-0.100417177000157,3.51852142809106));
#33144=CARTESIAN_POINT('Ctrl Pts',(19.3644992122339,0.350673329058588,3.65513271950473));
#33145=CARTESIAN_POINT('Ctrl Pts',(19.4122150482967,0.479735122332443,4.10844094226069));
#33146=CARTESIAN_POINT('Ctrl Pts',(19.4599308843596,0.168248769032157,4.46216617689766));
#33147=CARTESIAN_POINT('Ctrl Pts',(19.5076467204224,-0.297743013815871,
4.39147710422109));
#33148=CARTESIAN_POINT('Ctrl Pts',(19.5553625564852,-0.490312813065352,
3.96128857502183));
#33149=CARTESIAN_POINT('Ctrl Pts',(19.603078392548,-0.232620797759261,3.56664935826393));
#33150=CARTESIAN_POINT('Ctrl Pts',(19.6507942286109,0.238690449241969,3.56996267500769));
#33151=CARTESIAN_POINT('Ctrl Pts',(19.6985100646737,0.490808633485035,3.96818593857384));
#33152=CARTESIAN_POINT('Ctrl Pts',(19.7462259007366,0.292209604061002,4.39562444172689));
#33153=CARTESIAN_POINT('Ctrl Pts',(19.7939417367994,-0.174729824492781,
4.45975512619968));
#33154=CARTESIAN_POINT('Ctrl Pts',(19.8416575728622,-0.481212499922896,
4.10168523844358));
#33155=CARTESIAN_POINT('Ctrl Pts',(19.8893734089251,-0.345789702982467,
3.65023692191923));
#33156=CARTESIAN_POINT('Ctrl Pts',(19.9370892449879,0.107175910646637,3.51998011832295));
#33157=CARTESIAN_POINT('Ctrl Pts',(19.9848050810508,0.461722480014006,3.83053541934297));
#33158=CARTESIAN_POINT('Ctrl Pts',(20.0325209171136,0.392257955100357,4.29670800504879));
#33159=CARTESIAN_POINT('Ctrl Pts',(20.0802367531764,-0.0374150865130887,
4.49041783929577));
#33160=CARTESIAN_POINT('Ctrl Pts',(20.1279525892393,-0.432744382500041,
4.23375285658289));
#33161=CARTESIAN_POINT('Ctrl Pts',(20.1756684253021,-0.430649333670284,
3.76246031529274));
#33162=CARTESIAN_POINT('Ctrl Pts',(20.223384261365,-0.033136228617316,3.50924504180455));
#33163=CARTESIAN_POINT('Ctrl Pts',(20.2711000974278,0.394908089060633,3.70680919012016));
#33164=CARTESIAN_POINT('Ctrl Pts',(20.3188159334906,0.460110046434968,4.17340395051402));
#33165=CARTESIAN_POINT('Ctrl Pts',(20.3665317695535,0.103149962306437,4.48116018402389));
#33166=CARTESIAN_POINT('Ctrl Pts',(20.4142476056163,-0.34923165553999,4.34628168153608));
#33167=CARTESIAN_POINT('Ctrl Pts',(20.4540108023354,-0.457800032585507,
3.97025345815189));
#33168=CARTESIAN_POINT('Ctrl Pts',(20.4858213597105,-0.325993724402262,
3.71529210935379));
#33169=CARTESIAN_POINT('Ctrl Pts',(20.509679277742,-0.15096738523986,3.59329490328468));
#33170=CARTESIAN_POINT('Ctrl Pts',(20.5335371957734,0.0630371972956549,
3.57102347342756));
#33171=CARTESIAN_POINT('Ctrl Pts',(20.5573951138048,0.260511246441404,3.65349437971329));
#33172=CARTESIAN_POINT('Ctrl Pts',(20.5812530318362,0.394877283734959,3.82077798440408));
#33173=CARTESIAN_POINT('Ctrl Pts',(20.6051109498677,0.432370081305563,4.03184236506754));
#33174=CARTESIAN_POINT('Ctrl Pts',(20.6289688678991,0.364303478986858,4.23514367899931));
#33175=CARTESIAN_POINT('Ctrl Pts',(20.6528267859305,0.207066376217976,4.38093363836299));
#33176=CARTESIAN_POINT('Ctrl Pts',(20.6766847039619,-0.000757290757721993,
4.43358147160167));
#33177=CARTESIAN_POINT('Ctrl Pts',(20.7005426219933,-0.208420567790133,
4.38020336888205));
#33178=CARTESIAN_POINT('Ctrl Pts',(20.7244005400248,-0.365106210756856,
4.23385701605743));
#33179=CARTESIAN_POINT('Ctrl Pts',(20.7482584580562,-0.432520392530856,
4.03032528343114));
#33180=CARTESIAN_POINT('Ctrl Pts',(20.7721163760876,-0.394167874571092,
3.81937870627435));
#33181=CARTESIAN_POINT('Ctrl Pts',(20.795974294119,-0.259432524437891,3.65259868360638));
#33182=CARTESIAN_POINT('Ctrl Pts',(20.8198322121504,-0.0612578225112809,
3.57076788979259));
#33183=CARTESIAN_POINT('Ctrl Pts',(20.8436901301819,0.151895538690754,3.5938959627232));
#33184=CARTESIAN_POINT('Ctrl Pts',(20.8675480482132,0.327906592802717,3.71632757520176));
#33185=CARTESIAN_POINT('Ctrl Pts',(20.8914059662447,0.423735399567132,3.90812480123879));
#33186=CARTESIAN_POINT('Ctrl Pts',(20.9152638842761,0.415949440063929,4.12238802732943));
#33187=CARTESIAN_POINT('Ctrl Pts',(20.9391218023075,0.30645246920106,4.30672404095661));
#33188=CARTESIAN_POINT('Ctrl Pts',(20.962979720339,0.122019544809087,4.41605767475162));
#33189=CARTESIAN_POINT('Ctrl Pts',(20.9868376383703,-0.0922504941031022,
4.42365387220386));
#33190=CARTESIAN_POINT('Ctrl Pts',(21.0106955564018,-0.28396276796243,4.32765515869354));
#33191=CARTESIAN_POINT('Ctrl Pts',(21.0345534744332,-0.40623841344949,4.15153583326342));
#33192=CARTESIAN_POINT('Ctrl Pts',(21.0584113924646,-0.429177699343215,
3.93836186909709));
#33193=CARTESIAN_POINT('Ctrl Pts',(21.082269310496,-0.347171348131155,3.74026010679315));
#33194=CARTESIAN_POINT('Ctrl Pts',(21.1061272285274,-0.180272145040548,
3.605671823621));
#33195=CARTESIAN_POINT('Ctrl Pts',(21.1299851465589,0.0307085077608185,
3.56750752082027));
#33196=CARTESIAN_POINT('Ctrl Pts',(21.1538430645903,0.234180094072738,3.63509941005724));
#33197=CARTESIAN_POINT('Ctrl Pts',(21.1777009826217,0.380388268371489,3.79191943321731));
#33198=CARTESIAN_POINT('Ctrl Pts',(21.2015589006531,0.433581149524578,3.99962082296209));
#33199=CARTESIAN_POINT('Ctrl Pts',(21.2254168186846,0.380751629084578,4.2074149318183));
#33200=CARTESIAN_POINT('Ctrl Pts',(21.2492747367159,0.234817963878357,4.36449043997717));
#33201=CARTESIAN_POINT('Ctrl Pts',(21.2731326547474,0.0314649101850846,
4.43243810704058));
#33202=CARTESIAN_POINT('Ctrl Pts',(21.2969905727788,-0.179582171132277,
4.39464287755545));
#33203=CARTESIAN_POINT('Ctrl Pts',(21.3208484908102,-0.346716519889314,
4.26034671465164));
#33204=CARTESIAN_POINT('Ctrl Pts',(21.3447064088417,-0.429069235164158,
4.0623886883135));
#33205=CARTESIAN_POINT('Ctrl Pts',(21.368564326873,-0.406502834830527,3.8491749282489));
#33206=CARTESIAN_POINT('Ctrl Pts',(21.3924222449045,-0.284535418465691,
3.67284200661995));
#33207=CARTESIAN_POINT('Ctrl Pts',(21.4162801629359,-0.0929913416969399,
3.5765081259772));
#33208=CARTESIAN_POINT('Ctrl Pts',(21.4401380809674,0.121291651150069,3.58372954422009));
#33209=CARTESIAN_POINT('Ctrl Pts',(21.4639959989987,0.305915531372611,3.69274042788069));
#33210=CARTESIAN_POINT('Ctrl Pts',(21.4878539170302,0.415734731202803,3.87688464650718));
#33211=CARTESIAN_POINT('Ctrl Pts',(21.5117118350615,0.423895464867194,4.09113392265755));
#33212=CARTESIAN_POINT('Ctrl Pts',(21.535569753093,0.328402210690932,4.28309847227994));
#33213=CARTESIAN_POINT('Ctrl Pts',(21.5594276711244,0.152605670504114,4.40583773398234));
#33214=CARTESIAN_POINT('Ctrl Pts',(21.5832855891559,-0.0605071130159612,
4.42933861492812));
#33215=CARTESIAN_POINT('Ctrl Pts',(21.6071435071872,-0.258824259222961,
4.34785450957493));
#33216=CARTESIAN_POINT('Ctrl Pts',(21.6310014252187,-0.39385182381868,4.18131050126406));
#33217=CARTESIAN_POINT('Ctrl Pts',(21.6548593432501,-0.432571889182456,
3.97043113659525));
#33218=CARTESIAN_POINT('Ctrl Pts',(21.6787172612815,-0.365516344619441,
3.76678216446856));
#33219=CARTESIAN_POINT('Ctrl Pts',(21.702575179313,-0.209082097331647,3.62016130585559));
#33220=CARTESIAN_POINT('Ctrl Pts',(21.7264330973443,-0.00152158196427748,
3.56642135455923));
#33221=CARTESIAN_POINT('Ctrl Pts',(21.7502910153758,0.206411001640417,3.61870319251831));
#33222=CARTESIAN_POINT('Ctrl Pts',(21.7741489334072,0.363870472821225,3.76422248622317));
#33223=CARTESIAN_POINT('Ctrl Pts',(21.7980068514386,0.432353701764573,3.96739580449697));
#33224=CARTESIAN_POINT('Ctrl Pts',(21.82186476947,0.395114673548107,4.17854173669174));
#33225=CARTESIAN_POINT('Ctrl Pts',(21.8457226875014,0.261259344941517,4.3460293508861));
#33226=CARTESIAN_POINT('Ctrl Pts',(21.8695806055329,0.0635189899350569,
4.42890336313855));
#33227=CARTESIAN_POINT('Ctrl Pts',(21.8934385235643,-0.14975348833307,4.40689882001058));
#33228=CARTESIAN_POINT('Ctrl Pts',(21.9172964415957,-0.326407159500644,
4.28539643168872));
#33229=CARTESIAN_POINT('Ctrl Pts',(21.9411543596271,-0.423245389017799,
4.09410684177624));
#33230=CARTESIAN_POINT('Ctrl Pts',(21.9650122776585,-0.416588591947193,
3.87980556563057));
#33231=CARTESIAN_POINT('Ctrl Pts',(21.98887019569,-0.30806453650007,3.69489510271888));
#33232=CARTESIAN_POINT('Ctrl Pts',(22.0127281137213,-0.12421031036921,3.58459109808296));
#33233=CARTESIAN_POINT('Ctrl Pts',(22.0365860317528,0.0900167200678817,
3.57586588547707));
#33234=CARTESIAN_POINT('Ctrl Pts',(22.0604439497842,0.282232210442068,3.67085301705332));
#33235=CARTESIAN_POINT('Ctrl Pts',(22.0843018678157,0.405434237512275,3.8463255517439));
#33236=CARTESIAN_POINT('Ctrl Pts',(22.108159785847,0.429496549703537,4.05937567504088));
#33237=CARTESIAN_POINT('Ctrl Pts',(22.1320177038785,0.348535256241736,4.25790682842971));
#33238=CARTESIAN_POINT('Ctrl Pts',(22.1558756219099,0.182347598717988,4.39337273702606));
#33239=CARTESIAN_POINT('Ctrl Pts',(22.1797335399413,-0.0284290137391457,
4.43264829616218));
#33240=CARTESIAN_POINT('Ctrl Pts',(22.2035914579727,-0.232253957950086,
4.36612956178204));
#33241=CARTESIAN_POINT('Ctrl Pts',(22.2274493760041,-0.379286482964224,
4.21008217638027));
#33242=CARTESIAN_POINT('Ctrl Pts',(22.2513072940356,-0.433573131350875,
4.00266397632408));
#33243=CARTESIAN_POINT('Ctrl Pts',(22.275165212067,-0.381839338801546,3.79459436150246));
#33244=CARTESIAN_POINT('Ctrl Pts',(22.2990231300984,-0.236735426869051,
3.63675202040985));
#33245=CARTESIAN_POINT('Ctrl Pts',(22.3228810481298,-0.0337432544318164,
3.56773370504276));
#33246=CARTESIAN_POINT('Ctrl Pts',(22.3467389661613,0.177500062688638,3.60441627341574));
#33247=CARTESIAN_POINT('Ctrl Pts',(22.3705968841926,0.345339779804043,3.73782983856348));
#33248=CARTESIAN_POINT('Ctrl Pts',(22.3944548022241,0.428734513273282,3.93535114928888));
#33249=CARTESIAN_POINT('Ctrl Pts',(22.4183127202555,0.407291980919218,4.1486808655136));
#33250=CARTESIAN_POINT('Ctrl Pts',(22.4421706382869,0.286255462618544,4.32565405918856));
#33251=CARTESIAN_POINT('Ctrl Pts',(22.4660285563183,0.0952216904214238,
4.42299596654013));
#33252=CARTESIAN_POINT('Ctrl Pts',(22.4898864743497,-0.119096386717928,
4.41690383452019));
#33253=CARTESIAN_POINT('Ctrl Pts',(22.5137443923812,-0.304292138366774,
4.30886736509782));
#33254=CARTESIAN_POINT('Ctrl Pts',(22.5376023104126,-0.415080201412036,
4.12530439950267));
#33255=CARTESIAN_POINT('Ctrl Pts',(22.561460228444,-0.424369795825249,3.91110111771763));
#33256=CARTESIAN_POINT('Ctrl Pts',(22.5853181464754,-0.329889515310188,
3.71863599132299));
#33257=CARTESIAN_POINT('Ctrl Pts',(22.6091760645068,-0.154742073939436,
3.59497211022641));
#33258=CARTESIAN_POINT('Ctrl Pts',(22.6330339825383,0.0582436639512456,
3.57034842802071));
#33259=CARTESIAN_POINT('Ctrl Pts',(22.6568919005697,0.256987911016647,3.65078654733876));
#33260=CARTESIAN_POINT('Ctrl Pts',(22.6807498186011,0.39289034562191,3.81661632308649));
#33261=CARTESIAN_POINT('Ctrl Pts',(22.7046077366325,0.432722782933869,4.02728943245291));
#33262=CARTESIAN_POINT('Ctrl Pts',(22.7284656546639,0.366738191089385,4.2312875884069));
#33263=CARTESIAN_POINT('Ctrl Pts',(22.7523235726953,0.211084664509997,4.37873330099785));
#33264=CARTESIAN_POINT('Ctrl Pts',(22.7761814907268,0.00379901600965994,
4.43356145647204));
#33265=CARTESIAN_POINT('Ctrl Pts',(22.8000394087582,-0.204384723485633,
4.3823852668741));
#33266=CARTESIAN_POINT('Ctrl Pts',(22.8238973267896,-0.36265185203719,4.2376794731));
#33267=CARTESIAN_POINT('Ctrl Pts',(22.8398026054772,-0.408954280604672,
4.10250106973657));
#33268=CARTESIAN_POINT('Ctrl Pts',(22.847755244821,-0.414526965927561,4.03345758723954));
#33269=CARTESIAN_POINT('',(22.8,-0.592174260192535,4.04779597854866));
#33270=CARTESIAN_POINT('Ctrl Pts',(22.8,-0.19576256658266,4.36695865185836));
#33271=CARTESIAN_POINT('Ctrl Pts',(22.8,-0.195886593570853,4.36694806728808));
#33272=CARTESIAN_POINT('Ctrl Pts',(22.8,-0.196010613870461,4.36693742279878));
#33273=CARTESIAN_POINT('Ctrl Pts',(22.8,-0.196134627427637,4.36692671841166));
#33274=CARTESIAN_POINT('Ctrl Pts',(22.8,-0.216622178843513,4.36515830948628));
#33275=CARTESIAN_POINT('Ctrl Pts',(22.8,-0.236921239981942,4.36175743074964));
#33276=CARTESIAN_POINT('Ctrl Pts',(22.8,-0.256857422940798,4.35688458679081));
#33277=CARTESIAN_POINT('Ctrl Pts',(22.8,-0.271809560159941,4.35322995382169));
#33278=CARTESIAN_POINT('Ctrl Pts',(22.8,-0.286558947067823,4.34874691155445));
#33279=CARTESIAN_POINT('Ctrl Pts',(22.8,-0.301048271828705,4.34349077646485));
#33280=CARTESIAN_POINT('Ctrl Pts',(22.8,-0.310003423377303,4.3402422133286));
#33281=CARTESIAN_POINT('Ctrl Pts',(22.8,-0.318859482942331,4.33669811041118));
#33282=CARTESIAN_POINT('Ctrl Pts',(22.8,-0.327604744452034,4.33286912874946));
#33283=CARTESIAN_POINT('Ctrl Pts',(22.8,-0.333457186121174,4.33030672489195));
#33284=CARTESIAN_POINT('Ctrl Pts',(22.8,-0.33926207870774,4.32761569029118));
#33285=CARTESIAN_POINT('Ctrl Pts',(22.8,-0.345009487597299,4.32480202294401));
#33286=CARTESIAN_POINT('Ctrl Pts',(22.8,-0.365309066997251,4.31486428146495));
#33287=CARTESIAN_POINT('Ctrl Pts',(22.8,-0.384828901796994,4.30343044333042));
#33288=CARTESIAN_POINT('Ctrl Pts',(22.8,-0.403416958856431,4.29067119823496));
#33289=CARTESIAN_POINT('Ctrl Pts',(22.8,-0.409874425773003,4.28623865303559));
#33290=CARTESIAN_POINT('Ctrl Pts',(22.8,-0.416219739836017,4.28164578247975));
#33291=CARTESIAN_POINT('Ctrl Pts',(22.8,-0.422447327171508,4.27689854297234));
#33292=CARTESIAN_POINT('Ctrl Pts',(22.8,-0.43500295340691,4.2673274905416));
#33293=CARTESIAN_POINT('Ctrl Pts',(22.8,-0.447079966647781,4.25712966465555));
#33294=CARTESIAN_POINT('Ctrl Pts',(22.8,-0.458660056443695,4.24636133358853));
#33295=CARTESIAN_POINT('Ctrl Pts',(22.8,-0.465333929961841,4.24015529539631));
#33296=CARTESIAN_POINT('Ctrl Pts',(22.8,-0.471842796551704,4.23375955955572));
#33297=CARTESIAN_POINT('Ctrl Pts',(22.8,-0.478183280583292,4.22718326898633));
#33298=CARTESIAN_POINT('Ctrl Pts',(22.8,-0.48330469601013,4.22187138494));
#33299=CARTESIAN_POINT('Ctrl Pts',(22.8,-0.488310096860405,4.21644792156372));
#33300=CARTESIAN_POINT('Ctrl Pts',(22.8,-0.49319389770791,4.21092357737429));
#33301=CARTESIAN_POINT('Ctrl Pts',(22.8,-0.509882204568999,4.19204648678071));
#33302=CARTESIAN_POINT('Ctrl Pts',(22.8,-0.525164669297395,4.17198027236651));
#33303=CARTESIAN_POINT('Ctrl Pts',(22.8,-0.538985569877159,4.15095378743758));
#33304=CARTESIAN_POINT('Ctrl Pts',(22.8,-0.553292287721507,4.12918820238033));
#33305=CARTESIAN_POINT('Ctrl Pts',(22.8,-0.566034197593199,4.10639346234103));
#33306=CARTESIAN_POINT('Ctrl Pts',(22.8,-0.577149101532509,4.08276767497818));
#33307=CARTESIAN_POINT('Ctrl Pts',(22.8,-0.582543745751794,4.07130084468266));
#33308=CARTESIAN_POINT('Ctrl Pts',(22.8,-0.587554988912119,4.05963744408228));
#33309=CARTESIAN_POINT('Ctrl Pts',(22.8,-0.592174260192535,4.04779597854866));
#33310=CARTESIAN_POINT('Ctrl Pts',(22.8,-0.592174260192532,4.04779597854869));
#33311=CARTESIAN_POINT('Ctrl Pts',(22.7920473606562,-0.584213376873468,
4.14642833911734));
#33312=CARTESIAN_POINT('Ctrl Pts',(22.7840947213124,-0.551140611244481,
4.24298318064208));
#33313=CARTESIAN_POINT('Ctrl Pts',(22.7761420819686,-0.496922031827459,
4.32571394759471));
#33314=CARTESIAN_POINT('Ctrl Pts',(22.7681894426248,-0.442703452410443,
4.40844471454734));
#33315=CARTESIAN_POINT('Ctrl Pts',(22.760236803281,-0.367339059205388,4.47735140692785));
#33316=CARTESIAN_POINT('Ctrl Pts',(22.7522841639372,-0.280089901523161,
4.52398941366922));
#33317=CARTESIAN_POINT('Ctrl Pts',(22.7444712463773,-0.194373644734646,
4.56980802634291));
#33318=CARTESIAN_POINT('Ctrl Pts',(22.7366583288174,-0.0971865673270821,
4.59413356703531));
#33319=CARTESIAN_POINT('Ctrl Pts',(22.7288454112575,-7.11440487624268E-7,
4.59414971000239));
#33320=CARTESIAN_POINT('Origin',(27.2,0.3,2.9));
#33321=CARTESIAN_POINT('',(29.2,0.3,3.04606079858305));
#33322=CARTESIAN_POINT('',(27.2,0.3,3.04606079858305));
#33323=CARTESIAN_POINT('',(23.3,0.3,3.04606079858305));
#33324=CARTESIAN_POINT('',(29.2,0.3,3.35));
#33325=CARTESIAN_POINT('',(29.2,0.3,2.9));
#33326=CARTESIAN_POINT('',(27.2,0.3,3.35));
#33327=CARTESIAN_POINT('',(27.2,0.3,3.35));
#33328=CARTESIAN_POINT('',(27.2,0.3,2.9));
#33329=CARTESIAN_POINT('Origin',(27.2,0.,3.125));
#33330=CARTESIAN_POINT('',(27.2,-0.3,3.04606079858305));
#33331=CARTESIAN_POINT('Origin',(27.2,0.,4.));
#33332=CARTESIAN_POINT('',(27.2,-0.3,3.35));
#33333=CARTESIAN_POINT('',(27.2,0.3,3.35));
#33334=CARTESIAN_POINT('',(27.2,-0.3,3.35));
#33335=CARTESIAN_POINT('Origin',(27.2,0.3,3.35));
#33336=CARTESIAN_POINT('',(29.2,-0.3,3.35));
#33337=CARTESIAN_POINT('',(29.2,0.3,3.35));
#33338=CARTESIAN_POINT('',(27.2,-0.3,3.35));
#33339=CARTESIAN_POINT('Origin',(27.2,-0.3,3.35));
#33340=CARTESIAN_POINT('',(29.2,-0.3,3.04606079858305));
#33341=CARTESIAN_POINT('',(23.3,-0.3,3.04606079858305));
#33342=CARTESIAN_POINT('',(29.2,-0.3,3.35));
#33343=CARTESIAN_POINT('Origin',(29.2,0.,3.125));
#33344=CARTESIAN_POINT('Origin',(29.2,0.,4.));
#33345=CARTESIAN_POINT('Origin',(23.3,0.,4.));
#33346=CARTESIAN_POINT('',(29.4,-1.22464679914735E-16,5.));
#33347=CARTESIAN_POINT('Origin',(29.4,0.,4.));
#33348=CARTESIAN_POINT('',(23.3,-1.22464679914735E-16,5.));
#33349=CARTESIAN_POINT('',(23.3,-1.22464679914735E-16,5.));
#33350=CARTESIAN_POINT('Origin',(23.3,0.,4.));
#33351=CARTESIAN_POINT('Origin',(29.4,0.,4.));
#33352=CARTESIAN_POINT('Origin',(22.8,0.,4.));
#33353=CARTESIAN_POINT('',(22.8,-1.65327317884893E-16,5.35));
#33354=CARTESIAN_POINT('Origin',(22.8,0.,4.));
#33355=CARTESIAN_POINT('Origin',(22.8,0.,4.));
#33356=CARTESIAN_POINT('Origin',(22.8,0.,4.));
#33357=CARTESIAN_POINT('',(23.3,-1.65327317884893E-16,5.35));
#33358=CARTESIAN_POINT('Origin',(23.3,0.,4.));
#33359=CARTESIAN_POINT('',(22.8,-1.65327317884893E-16,5.35));
#33360=CARTESIAN_POINT('Origin',(23.3,0.,4.));
#33361=CARTESIAN_POINT('Origin',(4.,0.,4.));
#33362=CARTESIAN_POINT('',(0.,0.,0.));
#33363=CARTESIAN_POINT('Origin',(24.7,0.,4.));
#33364=CARTESIAN_POINT('',(25.4,-1.23689326713883E-16,5.01));
#33365=CARTESIAN_POINT('Origin',(25.4,0.,4.));
#33366=CARTESIAN_POINT('',(24.7,-1.23689326713883E-16,5.01));
#33367=CARTESIAN_POINT('',(24.7,-1.23689326713883E-16,5.01));
#33368=CARTESIAN_POINT('Origin',(24.7,0.,4.));
#33369=CARTESIAN_POINT('Origin',(24.7,0.,4.));
#33370=CARTESIAN_POINT('',(25.4,-1.65327317884893E-16,5.35));
#33371=CARTESIAN_POINT('Origin',(25.4,0.,4.));
#33372=CARTESIAN_POINT('',(24.7,-1.65327317884893E-16,5.35));
#33373=CARTESIAN_POINT('',(24.7,-1.65327317884893E-16,5.35));
#33374=CARTESIAN_POINT('Origin',(24.7,0.,4.));
#33375=CARTESIAN_POINT('Origin',(25.4,0.,4.));
#33376=CARTESIAN_POINT('Origin',(24.7,0.,4.));
#33377=CARTESIAN_POINT('',(0.,0.,0.));
#33378=CARTESIAN_POINT('Origin',(25.8,0.99,4.));
#33379=CARTESIAN_POINT('',(25.6809411910021,0.99,4.17298843892006));
#33380=CARTESIAN_POINT('',(25.9190588089979,0.99,4.17298843892006));
#33381=CARTESIAN_POINT('',(25.4,0.99,4.17298843892006));
#33382=CARTESIAN_POINT('Origin',(25.8,0.99,4.));
#33383=CARTESIAN_POINT('Origin',(25.8,0.99,4.));
#33384=CARTESIAN_POINT('',(25.6809411910021,0.99,3.82701156107994));
#33385=CARTESIAN_POINT('',(25.59,1.005,4.));
#33386=CARTESIAN_POINT('Ctrl Pts',(25.6809411910021,0.989999999999999,3.82701156107994));
#33387=CARTESIAN_POINT('Ctrl Pts',(25.6701985776047,0.99129192197638,3.83440513468868));
#33388=CARTESIAN_POINT('Ctrl Pts',(25.6603122906273,0.992653949439047,3.84270286127439));
#33389=CARTESIAN_POINT('Ctrl Pts',(25.6329072257467,0.996748084390898,3.87010792615492));
#33390=CARTESIAN_POINT('Ctrl Pts',(25.6167579436671,0.999695893276376,3.89366983224072));
#33391=CARTESIAN_POINT('Ctrl Pts',(25.5953022060351,1.00385029472357,3.94538709536759));
#33392=CARTESIAN_POINT('Ctrl Pts',(25.59,1.005,3.97354876917015));
#33393=CARTESIAN_POINT('Ctrl Pts',(25.59,1.005,4.));
#33394=CARTESIAN_POINT('',(25.9190588089979,0.99,3.82701156107994));
#33395=CARTESIAN_POINT('Origin',(25.8,0.99,4.));
#33396=CARTESIAN_POINT('Ctrl Pts',(25.9190588089979,0.99,4.17298843892006));
#33397=CARTESIAN_POINT('Ctrl Pts',(25.9298014223953,0.991291921976381,4.16559486531132));
#33398=CARTESIAN_POINT('Ctrl Pts',(25.9396877093727,0.992653949439047,4.15729713872561));
#33399=CARTESIAN_POINT('Ctrl Pts',(25.9670927742533,0.996748084390898,4.12989207384508));
#33400=CARTESIAN_POINT('Ctrl Pts',(25.9832420563329,0.999695893276376,4.10633016775929));
#33401=CARTESIAN_POINT('Ctrl Pts',(26.0046977939649,1.00385029472357,4.05461290463241));
#33402=CARTESIAN_POINT('Ctrl Pts',(26.01,1.005,4.02645123082985));
#33403=CARTESIAN_POINT('Ctrl Pts',(26.01,1.005,3.97354876917015));
#33404=CARTESIAN_POINT('Ctrl Pts',(26.0046977939649,1.00385029472357,3.94538709536759));
#33405=CARTESIAN_POINT('Ctrl Pts',(25.9832420563329,0.999695893276376,3.89366983224072));
#33406=CARTESIAN_POINT('Ctrl Pts',(25.9670927742533,0.996748084390898,3.87010792615492));
#33407=CARTESIAN_POINT('Ctrl Pts',(25.9396877093727,0.992653949439047,3.84270286127439));
#33408=CARTESIAN_POINT('Ctrl Pts',(25.9298014223953,0.991291921976381,3.83440513468868));
#33409=CARTESIAN_POINT('Ctrl Pts',(25.9190588089979,0.99,3.82701156107994));
#33410=CARTESIAN_POINT('Ctrl Pts',(25.59,1.005,4.));
#33411=CARTESIAN_POINT('Ctrl Pts',(25.59,1.005,4.02645123082985));
#33412=CARTESIAN_POINT('Ctrl Pts',(25.5953022060351,1.00385029472357,4.05461290463241));
#33413=CARTESIAN_POINT('Ctrl Pts',(25.6167579436671,0.999695893276376,4.10633016775929));
#33414=CARTESIAN_POINT('Ctrl Pts',(25.6329072257467,0.996748084390898,4.12989207384508));
#33415=CARTESIAN_POINT('Ctrl Pts',(25.6603122906273,0.992653949439047,4.15729713872561));
#33416=CARTESIAN_POINT('Ctrl Pts',(25.6701985776047,0.991291921976381,4.16559486531132));
#33417=CARTESIAN_POINT('Ctrl Pts',(25.6809411910021,0.99,4.17298843892006));
#33418=CARTESIAN_POINT('',(25.59,1.5,4.));
#33419=CARTESIAN_POINT('',(25.59,0.99,4.));
#33420=CARTESIAN_POINT('',(25.8,1.48522725533839,4.21));
#33421=CARTESIAN_POINT('Ctrl Pts',(25.8,1.48522725533839,4.21));
#33422=CARTESIAN_POINT('Ctrl Pts',(25.7735944730755,1.48522725533839,4.21));
#33423=CARTESIAN_POINT('Ctrl Pts',(25.7454529259093,1.48600415954412,4.2047157372696));
#33424=CARTESIAN_POINT('Ctrl Pts',(25.6937237310949,1.48880073282317,4.18327376303633));
#33425=CARTESIAN_POINT('Ctrl Pts',(25.670133075872,1.49077897157582,4.16711792397039));
#33426=CARTESIAN_POINT('Ctrl Pts',(25.632882321789,1.49448481141327,4.12986716988737));
#33427=CARTESIAN_POINT('Ctrl Pts',(25.6167262899986,1.49645455657129,4.10627640830577));
#33428=CARTESIAN_POINT('Ctrl Pts',(25.5952841751738,1.49923165515646,4.0545468514059));
#33429=CARTESIAN_POINT('Ctrl Pts',(25.59,1.5,4.02640517850928));
#33430=CARTESIAN_POINT('Ctrl Pts',(25.59,1.5,4.));
#33431=CARTESIAN_POINT('Ctrl Pts',(25.59,1.5,4.));
#33432=CARTESIAN_POINT('Ctrl Pts',(25.59,1.5,3.97359482149072));
#33433=CARTESIAN_POINT('Ctrl Pts',(25.5952841751738,1.49923165515646,3.9454531485941));
#33434=CARTESIAN_POINT('Ctrl Pts',(25.6167262899986,1.49645455657129,3.89372359169423));
#33435=CARTESIAN_POINT('Ctrl Pts',(25.632882321789,1.49448481141327,3.87013283011263));
#33436=CARTESIAN_POINT('Ctrl Pts',(25.670133075872,1.49077897157582,3.83288207602961));
#33437=CARTESIAN_POINT('Ctrl Pts',(25.6937237310949,1.48880073282317,3.81672623696366));
#33438=CARTESIAN_POINT('Ctrl Pts',(25.7454529259093,1.48600415954412,3.7952842627304));
#33439=CARTESIAN_POINT('Ctrl Pts',(25.7735944730755,1.48522725533839,3.79));
#33440=CARTESIAN_POINT('Ctrl Pts',(25.8264055269245,1.48522725533839,3.79));
#33441=CARTESIAN_POINT('Ctrl Pts',(25.8545470740907,1.48600415954412,3.7952842627304));
#33442=CARTESIAN_POINT('Ctrl Pts',(25.9062762689051,1.48880073282317,3.81672623696367));
#33443=CARTESIAN_POINT('Ctrl Pts',(25.929866924128,1.49077897157582,3.83288207602961));
#33444=CARTESIAN_POINT('Ctrl Pts',(25.967117678211,1.49448481141327,3.87013283011263));
#33445=CARTESIAN_POINT('Ctrl Pts',(25.9832737100014,1.49645455657129,3.89372359169423));
#33446=CARTESIAN_POINT('Ctrl Pts',(26.0047158248262,1.49923165515646,3.9454531485941));
#33447=CARTESIAN_POINT('Ctrl Pts',(26.01,1.5,3.97359482149072));
#33448=CARTESIAN_POINT('Ctrl Pts',(26.01,1.5,4.02640517850928));
#33449=CARTESIAN_POINT('Ctrl Pts',(26.0047158248262,1.49923165515646,4.0545468514059));
#33450=CARTESIAN_POINT('Ctrl Pts',(25.9832737100014,1.49645455657129,4.10627640830577));
#33451=CARTESIAN_POINT('Ctrl Pts',(25.967117678211,1.49448481141327,4.12986716988737));
#33452=CARTESIAN_POINT('Ctrl Pts',(25.929866924128,1.49077897157582,4.16711792397039));
#33453=CARTESIAN_POINT('Ctrl Pts',(25.9062762689051,1.48880073282317,4.18327376303633));
#33454=CARTESIAN_POINT('Ctrl Pts',(25.8545470740907,1.48600415954412,4.20471573726959));
#33455=CARTESIAN_POINT('Ctrl Pts',(25.8264055269245,1.48522725533839,4.21));
#33456=CARTESIAN_POINT('Ctrl Pts',(25.8,1.48522725533839,4.21));
#33457=CARTESIAN_POINT('Origin',(25.8,0.99,4.));
#33458=CARTESIAN_POINT('',(25.4,0.99,3.82701156107994));
#33459=CARTESIAN_POINT('Origin',(25.4,0.,4.));
#33460=CARTESIAN_POINT('',(26.2,-1.23077003314309E-16,5.005));
#33461=CARTESIAN_POINT('Origin',(26.2,0.,4.));
#33462=CARTESIAN_POINT('',(25.4,-1.23077003314309E-16,5.005));
#33463=CARTESIAN_POINT('',(25.4,-1.23077003314309E-16,5.005));
#33464=CARTESIAN_POINT('Origin',(25.4,0.,4.));
#33465=CARTESIAN_POINT('Origin',(25.4,0.,4.));
#33466=CARTESIAN_POINT('',(26.2,-1.83697019872103E-16,5.5));
#33467=CARTESIAN_POINT('Origin',(26.2,0.,4.));
#33468=CARTESIAN_POINT('',(25.4,-1.83697019872103E-16,5.5));
#33469=CARTESIAN_POINT('',(25.4,-1.83697019872103E-16,5.5));
#33470=CARTESIAN_POINT('Origin',(25.4,0.,4.));
#33471=CARTESIAN_POINT('Origin',(26.2,0.,4.));
#33472=CARTESIAN_POINT('Origin',(25.4,0.,4.));
#33473=CARTESIAN_POINT('',(0.,0.,0.));
#33474=CARTESIAN_POINT('Origin',(28.7,0.,6.5));
#33475=CARTESIAN_POINT('',(28.8,-3.06161699786838E-17,6.75));
#33476=CARTESIAN_POINT('Origin',(28.8,0.,6.5));
#33477=CARTESIAN_POINT('',(29.4,3.06161699786838E-17,6.75));
#33478=CARTESIAN_POINT('',(28.7,-3.06161699786838E-17,6.75));
#33479=CARTESIAN_POINT('Origin',(29.4,0.,6.5));
#33480=CARTESIAN_POINT('Origin',(28.,0.99,4.));
#33481=CARTESIAN_POINT('',(27.844436508139,0.99,4.14106735979666));
#33482=CARTESIAN_POINT('',(28.155563491861,0.99,4.14106735979666));
#33483=CARTESIAN_POINT('',(27.,0.99,4.14106735979666));
#33484=CARTESIAN_POINT('Origin',(28.,0.99,4.));
#33485=CARTESIAN_POINT('Origin',(28.,0.99,4.));
#33486=CARTESIAN_POINT('',(27.844436508139,0.99,3.85893264020334));
#33487=CARTESIAN_POINT('',(27.79,1.,4.));
#33488=CARTESIAN_POINT('Ctrl Pts',(27.844436508139,0.99,3.85893264020334));
#33489=CARTESIAN_POINT('Ctrl Pts',(27.8287948476368,0.992457849824465,3.87618164330178));
#33490=CARTESIAN_POINT('Ctrl Pts',(27.815375956669,0.994938193049464,3.8970013568903));
#33491=CARTESIAN_POINT('Ctrl Pts',(27.7953025362756,0.998844492372413,3.94538588560165));
#33492=CARTESIAN_POINT('Ctrl Pts',(27.79,1.,3.97354792631755));
#33493=CARTESIAN_POINT('Ctrl Pts',(27.79,1.,4.));
#33494=CARTESIAN_POINT('',(28.155563491861,0.99,3.85893264020334));
#33495=CARTESIAN_POINT('Origin',(28.,0.99,4.));
#33496=CARTESIAN_POINT('Ctrl Pts',(28.155563491861,0.99,4.14106735979666));
#33497=CARTESIAN_POINT('Ctrl Pts',(28.1712051523632,0.992457849824465,4.12381835669823));
#33498=CARTESIAN_POINT('Ctrl Pts',(28.184624043331,0.994938193049464,4.1029986431097));
#33499=CARTESIAN_POINT('Ctrl Pts',(28.2046974637244,0.998844492372413,4.05461411439835));
#33500=CARTESIAN_POINT('Ctrl Pts',(28.21,1.,4.02645207368245));
#33501=CARTESIAN_POINT('Ctrl Pts',(28.21,1.,3.97354792631755));
#33502=CARTESIAN_POINT('Ctrl Pts',(28.2046974637244,0.998844492372413,3.94538588560165));
#33503=CARTESIAN_POINT('Ctrl Pts',(28.184624043331,0.994938193049464,3.8970013568903));
#33504=CARTESIAN_POINT('Ctrl Pts',(28.1712051523632,0.992457849824465,3.87618164330178));
#33505=CARTESIAN_POINT('Ctrl Pts',(28.155563491861,0.99,3.85893264020334));
#33506=CARTESIAN_POINT('Ctrl Pts',(27.79,1.,4.));
#33507=CARTESIAN_POINT('Ctrl Pts',(27.79,1.,4.02645207368245));
#33508=CARTESIAN_POINT('Ctrl Pts',(27.7953025362756,0.998844492372413,4.05461411439835));
#33509=CARTESIAN_POINT('Ctrl Pts',(27.815375956669,0.994938193049464,4.1029986431097));
#33510=CARTESIAN_POINT('Ctrl Pts',(27.8287948476368,0.992457849824465,4.12381835669823));
#33511=CARTESIAN_POINT('Ctrl Pts',(27.844436508139,0.99,4.14106735979666));
#33512=CARTESIAN_POINT('',(27.79,1.5,4.));
#33513=CARTESIAN_POINT('',(27.79,0.99,4.));
#33514=CARTESIAN_POINT('',(28.,1.48522725533839,4.21));
#33515=CARTESIAN_POINT('Ctrl Pts',(28.,1.48522725533839,4.21));
#33516=CARTESIAN_POINT('Ctrl Pts',(27.9735944730755,1.48522725533839,4.21));
#33517=CARTESIAN_POINT('Ctrl Pts',(27.9454529259093,1.48600415954412,4.20471573726959));
#33518=CARTESIAN_POINT('Ctrl Pts',(27.8937237310949,1.48880073282317,4.18327376303633));
#33519=CARTESIAN_POINT('Ctrl Pts',(27.870133075872,1.49077897157582,4.16711792397039));
#33520=CARTESIAN_POINT('Ctrl Pts',(27.832882321789,1.49448481141327,4.12986716988737));
#33521=CARTESIAN_POINT('Ctrl Pts',(27.8167262899986,1.49645455657129,4.10627640830576));
#33522=CARTESIAN_POINT('Ctrl Pts',(27.7952841751738,1.49923165515646,4.0545468514059));
#33523=CARTESIAN_POINT('Ctrl Pts',(27.79,1.5,4.02640517850928));
#33524=CARTESIAN_POINT('Ctrl Pts',(27.79,1.5,4.));
#33525=CARTESIAN_POINT('Ctrl Pts',(27.79,1.5,4.));
#33526=CARTESIAN_POINT('Ctrl Pts',(27.79,1.5,3.97359482149072));
#33527=CARTESIAN_POINT('Ctrl Pts',(27.7952841751738,1.49923165515646,3.9454531485941));
#33528=CARTESIAN_POINT('Ctrl Pts',(27.8167262899986,1.49645455657129,3.89372359169424));
#33529=CARTESIAN_POINT('Ctrl Pts',(27.832882321789,1.49448481141327,3.87013283011263));
#33530=CARTESIAN_POINT('Ctrl Pts',(27.870133075872,1.49077897157582,3.83288207602961));
#33531=CARTESIAN_POINT('Ctrl Pts',(27.8937237310949,1.48880073282317,3.81672623696367));
#33532=CARTESIAN_POINT('Ctrl Pts',(27.9454529259093,1.48600415954412,3.7952842627304));
#33533=CARTESIAN_POINT('Ctrl Pts',(27.9735944730755,1.48522725533839,3.79));
#33534=CARTESIAN_POINT('Ctrl Pts',(28.0264055269245,1.48522725533839,3.79));
#33535=CARTESIAN_POINT('Ctrl Pts',(28.0545470740907,1.48600415954412,3.7952842627304));
#33536=CARTESIAN_POINT('Ctrl Pts',(28.1062762689051,1.48880073282317,3.81672623696367));
#33537=CARTESIAN_POINT('Ctrl Pts',(28.129866924128,1.49077897157582,3.83288207602961));
#33538=CARTESIAN_POINT('Ctrl Pts',(28.167117678211,1.49448481141327,3.87013283011263));
#33539=CARTESIAN_POINT('Ctrl Pts',(28.1832737100014,1.49645455657129,3.89372359169424));
#33540=CARTESIAN_POINT('Ctrl Pts',(28.2047158248262,1.49923165515646,3.9454531485941));
#33541=CARTESIAN_POINT('Ctrl Pts',(28.21,1.5,3.97359482149072));
#33542=CARTESIAN_POINT('Ctrl Pts',(28.21,1.5,4.02640517850928));
#33543=CARTESIAN_POINT('Ctrl Pts',(28.2047158248262,1.49923165515646,4.0545468514059));
#33544=CARTESIAN_POINT('Ctrl Pts',(28.1832737100014,1.49645455657129,4.10627640830576));
#33545=CARTESIAN_POINT('Ctrl Pts',(28.167117678211,1.49448481141327,4.12986716988737));
#33546=CARTESIAN_POINT('Ctrl Pts',(28.129866924128,1.49077897157582,4.16711792397039));
#33547=CARTESIAN_POINT('Ctrl Pts',(28.1062762689051,1.48880073282317,4.18327376303633));
#33548=CARTESIAN_POINT('Ctrl Pts',(28.0545470740907,1.48600415954412,4.2047157372696));
#33549=CARTESIAN_POINT('Ctrl Pts',(28.0264055269245,1.48522725533839,4.21));
#33550=CARTESIAN_POINT('Ctrl Pts',(28.,1.48522725533839,4.21));
#33551=CARTESIAN_POINT('Origin',(28.,0.99,4.));
#33552=CARTESIAN_POINT('',(27.,0.99,3.85893264020334));
#33553=CARTESIAN_POINT('Origin',(26.9,-0.3,4.));
#33554=CARTESIAN_POINT('',(29.4,-0.3,2.5));
#33555=CARTESIAN_POINT('',(29.4,-0.3,3.04606079858305));
#33556=CARTESIAN_POINT('',(29.4,-0.3,4.));
#33557=CARTESIAN_POINT('',(28.8,-0.3,2.5));
#33558=CARTESIAN_POINT('',(26.9,-0.3,2.5));
#33559=CARTESIAN_POINT('',(28.8,-0.3,2.53030615433009));
#33560=CARTESIAN_POINT('',(28.8,-0.3,4.));
#33561=CARTESIAN_POINT('',(27.,-0.3,2.53030615433009));
#33562=CARTESIAN_POINT('',(27.,-0.3,2.53030615433009));
#33563=CARTESIAN_POINT('',(27.,-0.3,3.04606079858305));
#33564=CARTESIAN_POINT('',(27.,-0.3,4.));
#33565=CARTESIAN_POINT('',(27.,-0.3,3.04606079858305));
#33566=CARTESIAN_POINT('Origin',(26.9,-0.3,2.5));
#33567=CARTESIAN_POINT('',(29.4,0.3,2.5));
#33568=CARTESIAN_POINT('',(29.4,-0.15,2.5));
#33569=CARTESIAN_POINT('',(28.8,0.3,2.5));
#33570=CARTESIAN_POINT('',(26.9,0.3,2.5));
#33571=CARTESIAN_POINT('',(28.8,-0.15,2.5));
#33572=CARTESIAN_POINT('Origin',(26.9,0.3,2.5));
#33573=CARTESIAN_POINT('',(29.4,0.3,3.04606079858305));
#33574=CARTESIAN_POINT('',(29.4,0.3,3.25));
#33575=CARTESIAN_POINT('',(27.,0.3,3.04606079858305));
#33576=CARTESIAN_POINT('',(27.,0.3,3.04606079858305));
#33577=CARTESIAN_POINT('',(27.,0.3,2.53030615433009));
#33578=CARTESIAN_POINT('',(27.,0.3,3.25));
#33579=CARTESIAN_POINT('',(28.8,0.3,2.53030615433009));
#33580=CARTESIAN_POINT('',(27.,0.3,2.53030615433009));
#33581=CARTESIAN_POINT('',(28.8,0.3,3.25));
#33582=CARTESIAN_POINT('Origin',(29.4,0.,4.));
#33583=CARTESIAN_POINT('',(29.4,-4.28626379701574E-16,7.5));
#33584=CARTESIAN_POINT('Origin',(29.4,0.,4.));
#33585=CARTESIAN_POINT('Origin',(29.4,0.,4.));
#33586=CARTESIAN_POINT('Origin',(28.8,0.,4.));
#33587=CARTESIAN_POINT('',(28.8,-4.28626379701574E-16,7.5));
#33588=CARTESIAN_POINT('Origin',(28.8,0.,4.));
#33589=CARTESIAN_POINT('Origin',(28.8,0.,4.));
#33590=CARTESIAN_POINT('Origin',(28.8,0.,4.));
#33591=CARTESIAN_POINT('',(28.8,-4.28626379701574E-16,7.5));
#33592=CARTESIAN_POINT('Origin',(27.,0.,4.));
#33593=CARTESIAN_POINT('Origin',(27.,0.,4.));
#33594=CARTESIAN_POINT('Origin',(27.,0.,4.));
#33595=CARTESIAN_POINT('Origin',(27.,0.,4.));
#33596=CARTESIAN_POINT('Origin',(27.,0.,4.));
#33597=CARTESIAN_POINT('',(0.,0.,0.));
#33598=CARTESIAN_POINT('Origin',(29.4,0.,6.5));
#33599=CARTESIAN_POINT('',(31.03,-4.04133443718627E-17,6.83));
#33600=CARTESIAN_POINT('Origin',(31.03,0.,6.5));
#33601=CARTESIAN_POINT('',(29.4,-4.04133443718627E-17,6.83));
#33602=CARTESIAN_POINT('',(29.4,-4.04133443718627E-17,6.83));
#33603=CARTESIAN_POINT('Origin',(29.4,0.,6.5));
#33604=CARTESIAN_POINT('Origin',(29.4,0.,6.5));
#33605=CARTESIAN_POINT('',(31.03,-4.89858719658942E-17,6.9));
#33606=CARTESIAN_POINT('Origin',(31.03,0.,6.5));
#33607=CARTESIAN_POINT('',(29.4,-4.89858719658942E-17,6.9));
#33608=CARTESIAN_POINT('',(29.4,-4.89858719658942E-17,6.9));
#33609=CARTESIAN_POINT('Origin',(29.4,0.,6.5));
#33610=CARTESIAN_POINT('Origin',(31.03,0.,6.5));
#33611=CARTESIAN_POINT('Origin',(29.4,0.,6.5));
#33612=CARTESIAN_POINT('',(0.,0.,0.));
#33613=CARTESIAN_POINT('Origin',(29.4,0.,6.5));
#33614=CARTESIAN_POINT('',(31.,-4.95981953654678E-17,6.905));
#33615=CARTESIAN_POINT('Origin',(31.,0.,6.5));
#33616=CARTESIAN_POINT('',(29.4,-4.95981953654678E-17,6.905));
#33617=CARTESIAN_POINT('',(29.4,-4.95981953654678E-17,6.905));
#33618=CARTESIAN_POINT('Origin',(29.4,0.,6.5));
#33619=CARTESIAN_POINT('Origin',(29.4,0.,6.5));
#33620=CARTESIAN_POINT('',(31.,-1.10218211923262E-16,7.4));
#33621=CARTESIAN_POINT('Origin',(31.,0.,6.5));
#33622=CARTESIAN_POINT('',(29.4,-1.10218211923262E-16,7.4));
#33623=CARTESIAN_POINT('',(29.4,-1.10218211923262E-16,7.4));
#33624=CARTESIAN_POINT('Origin',(29.4,0.,6.5));
#33625=CARTESIAN_POINT('Origin',(31.,0.,6.5));
#33626=CARTESIAN_POINT('Origin',(29.4,0.,6.5));
#33627=CARTESIAN_POINT('',(0.,0.,0.));
#33628=CARTESIAN_POINT('Origin',(-1.,0.,0.35));
#33629=CARTESIAN_POINT('',(-1.,-0.26,0.6));
#33630=CARTESIAN_POINT('',(-1.,-0.3,0.56));
#33631=CARTESIAN_POINT('',(-1.,-0.2675,0.5925));
#33632=CARTESIAN_POINT('',(-1.,0.26,0.6));
#33633=CARTESIAN_POINT('',(-1.,0.,0.6));
#33634=CARTESIAN_POINT('',(-1.,0.3,0.56));
#33635=CARTESIAN_POINT('',(-1.,0.2675,0.5925));
#33636=CARTESIAN_POINT('',(-1.,0.3,0.04));
#33637=CARTESIAN_POINT('',(-1.,0.3,0.175));
#33638=CARTESIAN_POINT('',(-1.,0.26,0.));
#33639=CARTESIAN_POINT('',(-1.,0.2925,0.0325));
#33640=CARTESIAN_POINT('',(-1.,-0.26,0.));
#33641=CARTESIAN_POINT('',(-1.,0.,0.));
#33642=CARTESIAN_POINT('',(-1.,-0.3,0.04));
#33643=CARTESIAN_POINT('',(-1.,-0.2925,0.0325));
#33644=CARTESIAN_POINT('',(-1.,-0.3,0.175));
#33645=CARTESIAN_POINT('Origin',(0.75,0.28,0.02));
#33646=CARTESIAN_POINT('',(1.,0.3,0.04));
#33647=CARTESIAN_POINT('',(0.75,0.3,0.04));
#33648=CARTESIAN_POINT('',(1.,0.26,0.));
#33649=CARTESIAN_POINT('',(1.,0.2925,0.0325));
#33650=CARTESIAN_POINT('',(0.75,0.26,0.));
#33651=CARTESIAN_POINT('Origin',(1.5,0.3,0.));
#33652=CARTESIAN_POINT('',(1.,0.3,0.56));
#33653=CARTESIAN_POINT('',(0.75,0.3,0.56));
#33654=CARTESIAN_POINT('',(1.,0.3,0.175));
#33655=CARTESIAN_POINT('Origin',(0.75,0.28,0.58));
#33656=CARTESIAN_POINT('',(1.,0.26,0.6));
#33657=CARTESIAN_POINT('',(0.75,0.26,0.6));
#33658=CARTESIAN_POINT('',(1.,0.2675,0.5925));
#33659=CARTESIAN_POINT('Origin',(0.,0.,0.6));
#33660=CARTESIAN_POINT('',(1.,-0.26,0.6));
#33661=CARTESIAN_POINT('',(-0.75,-0.26,0.6));
#33662=CARTESIAN_POINT('',(1.,0.,0.6));
#33663=CARTESIAN_POINT('Origin',(1.,0.,0.35));
#33664=CARTESIAN_POINT('',(1.,-0.26,0.));
#33665=CARTESIAN_POINT('',(1.,-0.3,0.04));
#33666=CARTESIAN_POINT('',(1.,-0.2925,0.0325));
#33667=CARTESIAN_POINT('',(1.,0.,0.));
#33668=CARTESIAN_POINT('',(1.,-0.3,0.56));
#33669=CARTESIAN_POINT('',(1.,-0.2675,0.5925));
#33670=CARTESIAN_POINT('',(1.,-0.3,0.175));
#33671=CARTESIAN_POINT('Origin',(0.,0.,0.));
#33672=CARTESIAN_POINT('',(-0.75,-0.26,0.));
#33673=CARTESIAN_POINT('Origin',(-0.75,-0.28,0.58));
#33674=CARTESIAN_POINT('',(-0.75,-0.3,0.56));
#33675=CARTESIAN_POINT('Origin',(-0.75,-0.28,0.02));
#33676=CARTESIAN_POINT('',(-0.75,-0.3,0.04));
#33677=CARTESIAN_POINT('Origin',(-1.5,-0.3,0.));
#33678=CARTESIAN_POINT('',(0.,0.,0.));
#33679=CARTESIAN_POINT('Origin',(0.0721687836487032,0.,-0.125));
#33680=CARTESIAN_POINT('',(0.0721687836487032,0.,-0.125));
#33681=CARTESIAN_POINT('',(0.144337567297406,0.,0.));
#33682=CARTESIAN_POINT('',(0.117710979560879,0.,-0.0461186027918559));
#33683=CARTESIAN_POINT('',(0.0721687836487032,-0.25,-0.125));
#33684=CARTESIAN_POINT('',(0.0721687836487032,0.,-0.125));
#33685=CARTESIAN_POINT('',(0.144337567297406,-0.25,0.));
#33686=CARTESIAN_POINT('',(0.144337567297406,-0.25,0.));
#33687=CARTESIAN_POINT('',(0.144337567297406,0.,0.));
#33688=CARTESIAN_POINT('Origin',(-0.0721687836487032,0.,-0.125));
#33689=CARTESIAN_POINT('',(-0.0721687836487032,0.,-0.125));
#33690=CARTESIAN_POINT('',(0.0739156081756484,0.,-0.125));
#33691=CARTESIAN_POINT('',(-0.0721687836487032,-0.25,-0.125));
#33692=CARTESIAN_POINT('',(-0.0721687836487032,0.,-0.125));
#33693=CARTESIAN_POINT('',(0.0721687836487032,-0.25,-0.125));
#33694=CARTESIAN_POINT('Origin',(-0.144337567297406,0.,-4.16333634234434E-17));
#33695=CARTESIAN_POINT('',(-0.144337567297406,0.,-1.76762539787485E-17));
#33696=CARTESIAN_POINT('',(-0.0987953713852306,0.,-0.0788813972081442));
#33697=CARTESIAN_POINT('',(-0.144337567297406,-0.25,-2.77555756156289E-17));
#33698=CARTESIAN_POINT('',(-0.144337567297406,0.,-1.76762539787485E-17));
#33699=CARTESIAN_POINT('',(-0.0721687836487032,-0.25,-0.125));
#33700=CARTESIAN_POINT('Origin',(-0.0721687836487033,0.,0.125));
#33701=CARTESIAN_POINT('',(-0.0721687836487033,0.,0.125));
#33702=CARTESIAN_POINT('',(-0.0627109795608791,0.,0.141381397208144));
#33703=CARTESIAN_POINT('',(-0.0721687836487033,-0.25,0.125));
#33704=CARTESIAN_POINT('',(-0.0721687836487033,0.,0.125));
#33705=CARTESIAN_POINT('',(-0.144337567297406,-0.25,-1.76762539787485E-17));
#33706=CARTESIAN_POINT('Origin',(0.0721687836487032,0.,0.125));
#33707=CARTESIAN_POINT('',(0.0721687836487032,0.,0.125));
#33708=CARTESIAN_POINT('',(0.146084391824352,0.,0.125));
#33709=CARTESIAN_POINT('',(0.0721687836487032,-0.25,0.125));
#33710=CARTESIAN_POINT('',(0.0721687836487032,0.,0.125));
#33711=CARTESIAN_POINT('',(-0.0721687836487033,-0.25,0.125));
#33712=CARTESIAN_POINT('Origin',(0.144337567297406,0.,0.));
#33713=CARTESIAN_POINT('',(0.153795371385231,0.,-0.0163813972081441));
#33714=CARTESIAN_POINT('',(0.0721687836487032,-0.25,0.125));
#33715=CARTESIAN_POINT('Origin',(0.,-0.25,0.));
#33716=CARTESIAN_POINT('Origin',(0.22,0.,0.));
#33717=CARTESIAN_POINT('',(-0.22,-8.67361737988404E-18,-2.69422295812418E-17));
#33718=CARTESIAN_POINT('Origin',(0.,0.,0.));
#33719=CARTESIAN_POINT('Origin',(0.,-0.015,0.));
#33720=CARTESIAN_POINT('',(-0.24505,-0.02505,-3.00099698131059E-17));
#33721=CARTESIAN_POINT('Origin',(0.,-0.02505,0.));
#33722=CARTESIAN_POINT('',(-0.235,-0.015,-2.87791997799628E-17));
#33723=CARTESIAN_POINT('Origin',(0.,-0.3775,0.));
#33724=CARTESIAN_POINT('',(-0.24505,-0.72995,3.00099698131059E-17));
#33725=CARTESIAN_POINT('Origin',(0.,-0.72995,0.));
#33726=CARTESIAN_POINT('',(-0.24505,-0.3775,-3.00099698131059E-17));
#33727=CARTESIAN_POINT('Origin',(0.,-0.7625,0.));
#33728=CARTESIAN_POINT('',(-0.175,-0.8,-2.14313189850787E-17));
#33729=CARTESIAN_POINT('Origin',(0.,-0.8,0.));
#33730=CARTESIAN_POINT('',(-0.2125,-0.7625,-2.60237444818813E-17));
#33731=CARTESIAN_POINT('Origin',(0.,-0.8,0.));
#33732=CARTESIAN_POINT('',(0.,0.,0.));
#33733=CARTESIAN_POINT('Origin',(0.,0.,0.));
#33734=CARTESIAN_POINT('',(-0.32,0.16,3.91886975727153E-17));
#33735=CARTESIAN_POINT('Origin',(0.,0.16,0.));
#33736=CARTESIAN_POINT('',(-0.32,0.,3.91886975727153E-17));
#33737=CARTESIAN_POINT('',(-0.32,0.,3.91886975727153E-17));
#33738=CARTESIAN_POINT('Origin',(0.,0.,0.));
#33739=CARTESIAN_POINT('Origin',(0.,0.,0.));
#33740=CARTESIAN_POINT('',(-0.6,0.16,7.34788079488412E-17));
#33741=CARTESIAN_POINT('Origin',(0.,0.16,0.));
#33742=CARTESIAN_POINT('',(-0.6,0.,7.34788079488412E-17));
#33743=CARTESIAN_POINT('',(-0.6,0.,7.34788079488412E-17));
#33744=CARTESIAN_POINT('Origin',(0.,0.,0.));
#33745=CARTESIAN_POINT('Origin',(0.,0.16,0.));
#33746=CARTESIAN_POINT('Origin',(0.,0.,0.));
#33747=CARTESIAN_POINT('',(0.,0.,0.));
#33748=CARTESIAN_POINT('Origin',(0.45,0.6,0.));
#33749=CARTESIAN_POINT('',(-0.45,0.6,-5.51091059616309E-17));
#33750=CARTESIAN_POINT('Origin',(0.,0.6,0.));
#33751=CARTESIAN_POINT('Origin',(0.,0.575,0.));
#33752=CARTESIAN_POINT('',(-0.5,0.55,-6.12323399573677E-17));
#33753=CARTESIAN_POINT('Origin',(0.,0.55,0.));
#33754=CARTESIAN_POINT('',(-0.475,0.575,-5.81707229594993E-17));
#33755=CARTESIAN_POINT('Origin',(0.,0.29,0.));
#33756=CARTESIAN_POINT('',(-0.5,0.0299999999999998,-6.12323399573677E-17));
#33757=CARTESIAN_POINT('Origin',(0.,0.0299999999999998,0.));
#33758=CARTESIAN_POINT('',(-0.5,0.29,-6.12323399573677E-17));
#33759=CARTESIAN_POINT('Origin',(0.,0.0150000000000001,0.));
#33760=CARTESIAN_POINT('',(-0.47,7.11236625150491E-17,-5.75583995599256E-17));
#33761=CARTESIAN_POINT('Origin',(0.,0.,0.));
#33762=CARTESIAN_POINT('',(-0.485,0.0150000000000001,-5.93953697586466E-17));
#33763=CARTESIAN_POINT('Origin',(0.32,0.,0.));
#33764=CARTESIAN_POINT('',(-0.32,-6.93889390390723E-18,-3.91886975727153E-17));
#33765=CARTESIAN_POINT('Origin',(0.,0.,0.));
#33766=CARTESIAN_POINT('Origin',(0.,-0.02,0.));
#33767=CARTESIAN_POINT('',(-0.2942,-0.0515999999999999,3.60291088309151E-17));
#33768=CARTESIAN_POINT('Origin',(0.,-0.0515999999999999,0.));
#33769=CARTESIAN_POINT('',(-0.31,-0.02,-3.7964050773568E-17));
#33770=CARTESIAN_POINT('Origin',(0.,-1.24,0.));
#33771=CARTESIAN_POINT('',(-0.2942,-2.4458,3.60291088309151E-17));
#33772=CARTESIAN_POINT('Origin',(0.,-2.4458,0.));
#33773=CARTESIAN_POINT('',(-0.2942,-1.24,-3.60291088309151E-17));
#33774=CARTESIAN_POINT('Origin',(0.,-2.47,0.));
#33775=CARTESIAN_POINT('',(-0.24,-2.5,-2.93915231795365E-17));
#33776=CARTESIAN_POINT('Origin',(0.,-2.5,0.));
#33777=CARTESIAN_POINT('',(-0.27,-2.47,-3.30654635769785E-17));
#33778=CARTESIAN_POINT('Origin',(0.,-2.5,0.));
#33779=CARTESIAN_POINT('Origin',(0.144337567297406,-0.6,-0.25));
#33780=CARTESIAN_POINT('',(0.288675134594813,-0.6,0.));
#33781=CARTESIAN_POINT('',(0.144337567297406,-0.6,-0.25));
#33782=CARTESIAN_POINT('',(0.288675134594813,-0.6,0.));
#33783=CARTESIAN_POINT('',(0.144337567297406,-0.96,-0.25));
#33784=CARTESIAN_POINT('',(0.144337567297406,-0.6,-0.25));
#33785=CARTESIAN_POINT('',(0.288675134594813,-0.96,0.));
#33786=CARTESIAN_POINT('',(0.288675134594813,-0.96,0.));
#33787=CARTESIAN_POINT('',(0.288675134594813,-0.6,0.));
#33788=CARTESIAN_POINT('Origin',(-0.144337567297406,-0.6,-0.25));
#33789=CARTESIAN_POINT('',(-0.144337567297406,-0.6,-0.25));
#33790=CARTESIAN_POINT('',(0.144337567297406,-0.6,-0.25));
#33791=CARTESIAN_POINT('',(-0.144337567297406,-0.96,-0.25));
#33792=CARTESIAN_POINT('',(-0.144337567297406,-0.6,-0.25));
#33793=CARTESIAN_POINT('',(0.144337567297406,-0.96,-0.25));
#33794=CARTESIAN_POINT('Origin',(-0.288675134594813,-0.6,-8.32667268468867E-17));
#33795=CARTESIAN_POINT('',(-0.288675134594813,-0.6,-3.53525079574969E-17));
#33796=CARTESIAN_POINT('',(-0.144337567297406,-0.6,-0.25));
#33797=CARTESIAN_POINT('',(-0.288675134594813,-0.96,-5.55111512312578E-17));
#33798=CARTESIAN_POINT('',(-0.288675134594813,-0.6,-3.53525079574969E-17));
#33799=CARTESIAN_POINT('',(-0.144337567297406,-0.96,-0.25));
#33800=CARTESIAN_POINT('Origin',(-0.144337567297407,-0.6,0.25));
#33801=CARTESIAN_POINT('',(-0.144337567297407,-0.6,0.25));
#33802=CARTESIAN_POINT('',(-0.288675134594813,-0.6,-3.53525079574969E-17));
#33803=CARTESIAN_POINT('',(-0.144337567297407,-0.96,0.25));
#33804=CARTESIAN_POINT('',(-0.144337567297407,-0.6,0.25));
#33805=CARTESIAN_POINT('',(-0.288675134594813,-0.96,-3.53525079574969E-17));
#33806=CARTESIAN_POINT('Origin',(0.144337567297406,-0.6,0.25));
#33807=CARTESIAN_POINT('',(0.144337567297406,-0.6,0.25));
#33808=CARTESIAN_POINT('',(-0.144337567297407,-0.6,0.25));
#33809=CARTESIAN_POINT('',(0.144337567297406,-0.96,0.25));
#33810=CARTESIAN_POINT('',(0.144337567297406,-0.6,0.25));
#33811=CARTESIAN_POINT('',(-0.144337567297407,-0.96,0.25));
#33812=CARTESIAN_POINT('Origin',(0.288675134594813,-0.6,0.));
#33813=CARTESIAN_POINT('',(0.144337567297406,-0.6,0.25));
#33814=CARTESIAN_POINT('',(0.144337567297406,-0.96,0.25));
#33815=CARTESIAN_POINT('Origin',(0.,-0.6,0.));
#33816=CARTESIAN_POINT('Origin',(0.,-0.96,0.));
#33817=CARTESIAN_POINT('',(0.,0.,0.));
#33818=CARTESIAN_POINT('',(0.,0.,0.));
#33819=CARTESIAN_POINT('',(0.,0.,0.));
#33820=CARTESIAN_POINT('',(0.,0.,0.));
#33821=CARTESIAN_POINT('',(0.,0.,0.));
#33822=CARTESIAN_POINT('',(0.,0.,0.));
#33823=CARTESIAN_POINT('',(0.,0.,0.));
#33824=CARTESIAN_POINT('',(0.,0.,0.));
#33825=CARTESIAN_POINT('',(1.,-7.8,2.2));
#33826=CARTESIAN_POINT('',(1.,-4.2,2.2));
#33827=CARTESIAN_POINT('',(21.,-7.8,2.2));
#33828=CARTESIAN_POINT('',(21.,-4.2,2.2));
#33829=CARTESIAN_POINT('',(0.,-6.,2.8));
#33830=CARTESIAN_POINT('',(2.,-6.,3.77));
#33831=CARTESIAN_POINT('',(8.,-6.,3.77));
#33832=CARTESIAN_POINT('',(14.,-6.,3.77));
#33833=CARTESIAN_POINT('',(20.,-6.,3.77));
#33834=CARTESIAN_POINT('',(3.,-2.4,0.));
#33835=CARTESIAN_POINT('',(3.,2.4,0.));
#33836=CARTESIAN_POINT('',(3.,0.,4.));
#33837=CARTESIAN_POINT('',(1.6,-2.1,4.));
#33838=CARTESIAN_POINT('',(1.6,2.1,4.));
#33839=CARTESIAN_POINT('',(1.6,0.,6.1));
#33840=CARTESIAN_POINT('',(24.,-3.5,0.));
#33841=CARTESIAN_POINT('',(24.,3.5,0.));
#33842=CARTESIAN_POINT('',(24.,0.,4.));
#33843=CARTESIAN_POINT('',(25.4,-2.6,4.));
#33844=CARTESIAN_POINT('',(25.4,2.6,4.));
#33845=CARTESIAN_POINT('',(25.4,0.,6.6));
#33846=CARTESIAN_POINT('',(4.7,-9.,2.4));
#33847=CARTESIAN_POINT('',(4.7,-3.,2.4));
#33848=CARTESIAN_POINT('',(22.3,-9.,2.4));
#33849=CARTESIAN_POINT('',(22.3,-3.,2.4));
#33850=CARTESIAN_POINT('',(0.,-9.,-1.));
#33851=CARTESIAN_POINT('',(8.,-9.,-0.58));
#33852=CARTESIAN_POINT('',(8.,-9.,1.2));
#33853=CARTESIAN_POINT('',(8.,-9.,1.3));
#33854=CARTESIAN_POINT('',(19.,-9.,-0.58));
#33855=CARTESIAN_POINT('',(19.,-9.,1.2));
#33856=CARTESIAN_POINT('',(19.,-9.,1.3));
#33857=CARTESIAN_POINT('',(0.,-0.9,-1.));
#33858=CARTESIAN_POINT('',(8.,-0.9,-0.58));
#33859=CARTESIAN_POINT('',(8.,-0.9,1.2));
#33860=CARTESIAN_POINT('',(8.,-0.9,1.3));
#33861=CARTESIAN_POINT('',(19.,-0.9,-0.58));
#33862=CARTESIAN_POINT('',(19.,-0.9,1.2));
#33863=CARTESIAN_POINT('',(19.,-0.9,1.3));
#33864=CARTESIAN_POINT('',(0.,0.,0.));
#33865=CARTESIAN_POINT('',(0.,0.,0.));
#33866=CARTESIAN_POINT('',(0.,0.,0.));
#33867=CARTESIAN_POINT('',(0.,0.,0.));
#33868=CARTESIAN_POINT('',(0.,0.,0.));
#33869=CARTESIAN_POINT('',(0.,0.,0.));
#33870=CARTESIAN_POINT('',(28.2,0.,3.35));
#33871=CARTESIAN_POINT('',(25.8,1.8,4.));
#33872=CARTESIAN_POINT('',(28.,1.8,4.));
#33873=CARTESIAN_POINT('',(31.03,0.,6.5));
#33874=CARTESIAN_POINT('',(31.19,0.,6.5));
#33875=CARTESIAN_POINT('',(0.,0.,0.));
#33876=CARTESIAN_POINT('',(-0.391709409685019,-1.24208747939982E-15,8.88178419700125E-16));
#33877=CARTESIAN_POINT('',(0.,-0.691066002949543,0.0601487617464257));
#33878=UNCERTAINTY_MEASURE_WITH_UNIT(LENGTH_MEASURE(0.001),#33982,
'DISTANCE_ACCURACY_VALUE',
'Maximum model space distance between geometric entities at asserted c
onnectivities');
#33879=UNCERTAINTY_MEASURE_WITH_UNIT(LENGTH_MEASURE(0.001),#33982,
'DISTANCE_ACCURACY_VALUE',
'Maximum model space distance between geometric entities at asserted c
onnectivities');
#33880=UNCERTAINTY_MEASURE_WITH_UNIT(LENGTH_MEASURE(0.001),#33982,
'DISTANCE_ACCURACY_VALUE',
'Maximum model space distance between geometric entities at asserted c
onnectivities');
#33881=UNCERTAINTY_MEASURE_WITH_UNIT(LENGTH_MEASURE(0.001),#33982,
'DISTANCE_ACCURACY_VALUE',
'Maximum model space distance between geometric entities at asserted c
onnectivities');
#33882=UNCERTAINTY_MEASURE_WITH_UNIT(LENGTH_MEASURE(0.001),#33982,
'DISTANCE_ACCURACY_VALUE',
'Maximum model space distance between geometric entities at asserted c
onnectivities');
#33883=UNCERTAINTY_MEASURE_WITH_UNIT(LENGTH_MEASURE(0.001),#33982,
'DISTANCE_ACCURACY_VALUE',
'Maximum model space distance between geometric entities at asserted c
onnectivities');
#33884=UNCERTAINTY_MEASURE_WITH_UNIT(LENGTH_MEASURE(0.001),#33982,
'DISTANCE_ACCURACY_VALUE',
'Maximum model space distance between geometric entities at asserted c
onnectivities');
#33885=UNCERTAINTY_MEASURE_WITH_UNIT(LENGTH_MEASURE(0.001),#33982,
'DISTANCE_ACCURACY_VALUE',
'Maximum model space distance between geometric entities at asserted c
onnectivities');
#33886=UNCERTAINTY_MEASURE_WITH_UNIT(LENGTH_MEASURE(0.001),#33982,
'DISTANCE_ACCURACY_VALUE',
'Maximum model space distance between geometric entities at asserted c
onnectivities');
#33887=UNCERTAINTY_MEASURE_WITH_UNIT(LENGTH_MEASURE(0.001),#33982,
'DISTANCE_ACCURACY_VALUE',
'Maximum model space distance between geometric entities at asserted c
onnectivities');
#33888=UNCERTAINTY_MEASURE_WITH_UNIT(LENGTH_MEASURE(0.001),#33982,
'DISTANCE_ACCURACY_VALUE',
'Maximum model space distance between geometric entities at asserted c
onnectivities');
#33889=UNCERTAINTY_MEASURE_WITH_UNIT(LENGTH_MEASURE(0.001),#33982,
'DISTANCE_ACCURACY_VALUE',
'Maximum model space distance between geometric entities at asserted c
onnectivities');
#33890=UNCERTAINTY_MEASURE_WITH_UNIT(LENGTH_MEASURE(0.001),#33982,
'DISTANCE_ACCURACY_VALUE',
'Maximum model space distance between geometric entities at asserted c
onnectivities');
#33891=UNCERTAINTY_MEASURE_WITH_UNIT(LENGTH_MEASURE(0.001),#33982,
'DISTANCE_ACCURACY_VALUE',
'Maximum model space distance between geometric entities at asserted c
onnectivities');
#33892=UNCERTAINTY_MEASURE_WITH_UNIT(LENGTH_MEASURE(0.001),#33982,
'DISTANCE_ACCURACY_VALUE',
'Maximum model space distance between geometric entities at asserted c
onnectivities');
#33893=UNCERTAINTY_MEASURE_WITH_UNIT(LENGTH_MEASURE(0.001),#33982,
'DISTANCE_ACCURACY_VALUE',
'Maximum model space distance between geometric entities at asserted c
onnectivities');
#33894=UNCERTAINTY_MEASURE_WITH_UNIT(LENGTH_MEASURE(0.001),#33982,
'DISTANCE_ACCURACY_VALUE',
'Maximum model space distance between geometric entities at asserted c
onnectivities');
#33895=UNCERTAINTY_MEASURE_WITH_UNIT(LENGTH_MEASURE(0.001),#33982,
'DISTANCE_ACCURACY_VALUE',
'Maximum model space distance between geometric entities at asserted c
onnectivities');
#33896=UNCERTAINTY_MEASURE_WITH_UNIT(LENGTH_MEASURE(0.001),#33982,
'DISTANCE_ACCURACY_VALUE',
'Maximum model space distance between geometric entities at asserted c
onnectivities');
#33897=UNCERTAINTY_MEASURE_WITH_UNIT(LENGTH_MEASURE(0.001),#33982,
'DISTANCE_ACCURACY_VALUE',
'Maximum model space distance between geometric entities at asserted c
onnectivities');
#33898=UNCERTAINTY_MEASURE_WITH_UNIT(LENGTH_MEASURE(0.001),#33982,
'DISTANCE_ACCURACY_VALUE',
'Maximum model space distance between geometric entities at asserted c
onnectivities');
#33899=UNCERTAINTY_MEASURE_WITH_UNIT(LENGTH_MEASURE(0.001),#33982,
'DISTANCE_ACCURACY_VALUE',
'Maximum model space distance between geometric entities at asserted c
onnectivities');
#33900=UNCERTAINTY_MEASURE_WITH_UNIT(LENGTH_MEASURE(0.001),#33982,
'DISTANCE_ACCURACY_VALUE',
'Maximum model space distance between geometric entities at asserted c
onnectivities');
#33901=UNCERTAINTY_MEASURE_WITH_UNIT(LENGTH_MEASURE(0.001),#33982,
'DISTANCE_ACCURACY_VALUE',
'Maximum model space distance between geometric entities at asserted c
onnectivities');
#33902=UNCERTAINTY_MEASURE_WITH_UNIT(LENGTH_MEASURE(0.001),#33982,
'DISTANCE_ACCURACY_VALUE',
'Maximum model space distance between geometric entities at asserted c
onnectivities');
#33903=UNCERTAINTY_MEASURE_WITH_UNIT(LENGTH_MEASURE(0.001),#33982,
'DISTANCE_ACCURACY_VALUE',
'Maximum model space distance between geometric entities at asserted c
onnectivities');
#33904=UNCERTAINTY_MEASURE_WITH_UNIT(LENGTH_MEASURE(0.001),#33982,
'DISTANCE_ACCURACY_VALUE',
'Maximum model space distance between geometric entities at asserted c
onnectivities');
#33905=UNCERTAINTY_MEASURE_WITH_UNIT(LENGTH_MEASURE(0.001),#33982,
'DISTANCE_ACCURACY_VALUE',
'Maximum model space distance between geometric entities at asserted c
onnectivities');
#33906=UNCERTAINTY_MEASURE_WITH_UNIT(LENGTH_MEASURE(0.001),#33982,
'DISTANCE_ACCURACY_VALUE',
'Maximum model space distance between geometric entities at asserted c
onnectivities');
#33907=UNCERTAINTY_MEASURE_WITH_UNIT(LENGTH_MEASURE(0.001),#33982,
'DISTANCE_ACCURACY_VALUE',
'Maximum model space distance between geometric entities at asserted c
onnectivities');
#33908=UNCERTAINTY_MEASURE_WITH_UNIT(LENGTH_MEASURE(0.001),#33982,
'DISTANCE_ACCURACY_VALUE',
'Maximum model space distance between geometric entities at asserted c
onnectivities');
#33909=UNCERTAINTY_MEASURE_WITH_UNIT(LENGTH_MEASURE(0.001),#33982,
'DISTANCE_ACCURACY_VALUE',
'Maximum model space distance between geometric entities at asserted c
onnectivities');
#33910=UNCERTAINTY_MEASURE_WITH_UNIT(LENGTH_MEASURE(0.001),#33982,
'DISTANCE_ACCURACY_VALUE',
'Maximum model space distance between geometric entities at asserted c
onnectivities');
#33911=UNCERTAINTY_MEASURE_WITH_UNIT(LENGTH_MEASURE(0.001),#33982,
'DISTANCE_ACCURACY_VALUE',
'Maximum model space distance between geometric entities at asserted c
onnectivities');
#33912=UNCERTAINTY_MEASURE_WITH_UNIT(LENGTH_MEASURE(0.001),#33982,
'DISTANCE_ACCURACY_VALUE',
'Maximum model space distance between geometric entities at asserted c
onnectivities');
#33913=UNCERTAINTY_MEASURE_WITH_UNIT(LENGTH_MEASURE(0.001),#33982,
'DISTANCE_ACCURACY_VALUE',
'Maximum model space distance between geometric entities at asserted c
onnectivities');
#33914=UNCERTAINTY_MEASURE_WITH_UNIT(LENGTH_MEASURE(0.001),#33982,
'DISTANCE_ACCURACY_VALUE',
'Maximum model space distance between geometric entities at asserted c
onnectivities');
#33915=UNCERTAINTY_MEASURE_WITH_UNIT(LENGTH_MEASURE(0.001),#33982,
'DISTANCE_ACCURACY_VALUE',
'Maximum model space distance between geometric entities at asserted c
onnectivities');
#33916=UNCERTAINTY_MEASURE_WITH_UNIT(LENGTH_MEASURE(0.001),#33982,
'DISTANCE_ACCURACY_VALUE',
'Maximum model space distance between geometric entities at asserted c
onnectivities');
#33917=UNCERTAINTY_MEASURE_WITH_UNIT(LENGTH_MEASURE(0.001),#33982,
'DISTANCE_ACCURACY_VALUE',
'Maximum model space distance between geometric entities at asserted c
onnectivities');
#33918=UNCERTAINTY_MEASURE_WITH_UNIT(LENGTH_MEASURE(0.001),#33982,
'DISTANCE_ACCURACY_VALUE',
'Maximum model space distance between geometric entities at asserted c
onnectivities');
#33919=UNCERTAINTY_MEASURE_WITH_UNIT(LENGTH_MEASURE(0.001),#33982,
'DISTANCE_ACCURACY_VALUE',
'Maximum model space distance between geometric entities at asserted c
onnectivities');
#33920=UNCERTAINTY_MEASURE_WITH_UNIT(LENGTH_MEASURE(0.001),#33982,
'DISTANCE_ACCURACY_VALUE',
'Maximum model space distance between geometric entities at asserted c
onnectivities');
#33921=UNCERTAINTY_MEASURE_WITH_UNIT(LENGTH_MEASURE(0.001),#33982,
'DISTANCE_ACCURACY_VALUE',
'Maximum model space distance between geometric entities at asserted c
onnectivities');
#33922=UNCERTAINTY_MEASURE_WITH_UNIT(LENGTH_MEASURE(0.001),#33982,
'DISTANCE_ACCURACY_VALUE',
'Maximum model space distance between geometric entities at asserted c
onnectivities');
#33923=UNCERTAINTY_MEASURE_WITH_UNIT(LENGTH_MEASURE(0.001),#33982,
'DISTANCE_ACCURACY_VALUE',
'Maximum model space distance between geometric entities at asserted c
onnectivities');
#33924=UNCERTAINTY_MEASURE_WITH_UNIT(LENGTH_MEASURE(0.001),#33982,
'DISTANCE_ACCURACY_VALUE',
'Maximum model space distance between geometric entities at asserted c
onnectivities');
#33925=UNCERTAINTY_MEASURE_WITH_UNIT(LENGTH_MEASURE(0.001),#33982,
'DISTANCE_ACCURACY_VALUE',
'Maximum model space distance between geometric entities at asserted c
onnectivities');
#33926=UNCERTAINTY_MEASURE_WITH_UNIT(LENGTH_MEASURE(0.001),#33982,
'DISTANCE_ACCURACY_VALUE',
'Maximum model space distance between geometric entities at asserted c
onnectivities');
#33927=UNCERTAINTY_MEASURE_WITH_UNIT(LENGTH_MEASURE(0.001),#33982,
'DISTANCE_ACCURACY_VALUE',
'Maximum model space distance between geometric entities at asserted c
onnectivities');
#33928=UNCERTAINTY_MEASURE_WITH_UNIT(LENGTH_MEASURE(0.001),#33982,
'DISTANCE_ACCURACY_VALUE',
'Maximum model space distance between geometric entities at asserted c
onnectivities');
#33929=UNCERTAINTY_MEASURE_WITH_UNIT(LENGTH_MEASURE(0.001),#33982,
'DISTANCE_ACCURACY_VALUE',
'Maximum model space distance between geometric entities at asserted c
onnectivities');
#33930=(
GEOMETRIC_REPRESENTATION_CONTEXT(3)
GLOBAL_UNCERTAINTY_ASSIGNED_CONTEXT((#33878))
GLOBAL_UNIT_ASSIGNED_CONTEXT((#33982,#33984,#33985))
REPRESENTATION_CONTEXT('','3D')
);
#33931=(
GEOMETRIC_REPRESENTATION_CONTEXT(3)
GLOBAL_UNCERTAINTY_ASSIGNED_CONTEXT((#33879))
GLOBAL_UNIT_ASSIGNED_CONTEXT((#33982,#33984,#33985))
REPRESENTATION_CONTEXT('','3D')
);
#33932=(
GEOMETRIC_REPRESENTATION_CONTEXT(3)
GLOBAL_UNCERTAINTY_ASSIGNED_CONTEXT((#33880))
GLOBAL_UNIT_ASSIGNED_CONTEXT((#33982,#33984,#33985))
REPRESENTATION_CONTEXT('','3D')
);
#33933=(
GEOMETRIC_REPRESENTATION_CONTEXT(3)
GLOBAL_UNCERTAINTY_ASSIGNED_CONTEXT((#33881))
GLOBAL_UNIT_ASSIGNED_CONTEXT((#33982,#33984,#33985))
REPRESENTATION_CONTEXT('','3D')
);
#33934=(
GEOMETRIC_REPRESENTATION_CONTEXT(3)
GLOBAL_UNCERTAINTY_ASSIGNED_CONTEXT((#33882))
GLOBAL_UNIT_ASSIGNED_CONTEXT((#33982,#33984,#33985))
REPRESENTATION_CONTEXT('','3D')
);
#33935=(
GEOMETRIC_REPRESENTATION_CONTEXT(3)
GLOBAL_UNCERTAINTY_ASSIGNED_CONTEXT((#33883))
GLOBAL_UNIT_ASSIGNED_CONTEXT((#33982,#33984,#33985))
REPRESENTATION_CONTEXT('','3D')
);
#33936=(
GEOMETRIC_REPRESENTATION_CONTEXT(3)
GLOBAL_UNCERTAINTY_ASSIGNED_CONTEXT((#33884))
GLOBAL_UNIT_ASSIGNED_CONTEXT((#33982,#33984,#33985))
REPRESENTATION_CONTEXT('','3D')
);
#33937=(
GEOMETRIC_REPRESENTATION_CONTEXT(3)
GLOBAL_UNCERTAINTY_ASSIGNED_CONTEXT((#33885))
GLOBAL_UNIT_ASSIGNED_CONTEXT((#33982,#33984,#33985))
REPRESENTATION_CONTEXT('','3D')
);
#33938=(
GEOMETRIC_REPRESENTATION_CONTEXT(3)
GLOBAL_UNCERTAINTY_ASSIGNED_CONTEXT((#33886))
GLOBAL_UNIT_ASSIGNED_CONTEXT((#33982,#33984,#33985))
REPRESENTATION_CONTEXT('','3D')
);
#33939=(
GEOMETRIC_REPRESENTATION_CONTEXT(3)
GLOBAL_UNCERTAINTY_ASSIGNED_CONTEXT((#33887))
GLOBAL_UNIT_ASSIGNED_CONTEXT((#33982,#33984,#33985))
REPRESENTATION_CONTEXT('','3D')
);
#33940=(
GEOMETRIC_REPRESENTATION_CONTEXT(3)
GLOBAL_UNCERTAINTY_ASSIGNED_CONTEXT((#33888))
GLOBAL_UNIT_ASSIGNED_CONTEXT((#33982,#33984,#33985))
REPRESENTATION_CONTEXT('','3D')
);
#33941=(
GEOMETRIC_REPRESENTATION_CONTEXT(3)
GLOBAL_UNCERTAINTY_ASSIGNED_CONTEXT((#33889))
GLOBAL_UNIT_ASSIGNED_CONTEXT((#33982,#33984,#33985))
REPRESENTATION_CONTEXT('','3D')
);
#33942=(
GEOMETRIC_REPRESENTATION_CONTEXT(3)
GLOBAL_UNCERTAINTY_ASSIGNED_CONTEXT((#33890))
GLOBAL_UNIT_ASSIGNED_CONTEXT((#33982,#33984,#33985))
REPRESENTATION_CONTEXT('','3D')
);
#33943=(
GEOMETRIC_REPRESENTATION_CONTEXT(3)
GLOBAL_UNCERTAINTY_ASSIGNED_CONTEXT((#33891))
GLOBAL_UNIT_ASSIGNED_CONTEXT((#33982,#33984,#33985))
REPRESENTATION_CONTEXT('','3D')
);
#33944=(
GEOMETRIC_REPRESENTATION_CONTEXT(3)
GLOBAL_UNCERTAINTY_ASSIGNED_CONTEXT((#33892))
GLOBAL_UNIT_ASSIGNED_CONTEXT((#33982,#33984,#33985))
REPRESENTATION_CONTEXT('','3D')
);
#33945=(
GEOMETRIC_REPRESENTATION_CONTEXT(3)
GLOBAL_UNCERTAINTY_ASSIGNED_CONTEXT((#33893))
GLOBAL_UNIT_ASSIGNED_CONTEXT((#33982,#33984,#33985))
REPRESENTATION_CONTEXT('','3D')
);
#33946=(
GEOMETRIC_REPRESENTATION_CONTEXT(3)
GLOBAL_UNCERTAINTY_ASSIGNED_CONTEXT((#33894))
GLOBAL_UNIT_ASSIGNED_CONTEXT((#33982,#33984,#33985))
REPRESENTATION_CONTEXT('','3D')
);
#33947=(
GEOMETRIC_REPRESENTATION_CONTEXT(3)
GLOBAL_UNCERTAINTY_ASSIGNED_CONTEXT((#33895))
GLOBAL_UNIT_ASSIGNED_CONTEXT((#33982,#33984,#33985))
REPRESENTATION_CONTEXT('','3D')
);
#33948=(
GEOMETRIC_REPRESENTATION_CONTEXT(3)
GLOBAL_UNCERTAINTY_ASSIGNED_CONTEXT((#33896))
GLOBAL_UNIT_ASSIGNED_CONTEXT((#33982,#33984,#33985))
REPRESENTATION_CONTEXT('','3D')
);
#33949=(
GEOMETRIC_REPRESENTATION_CONTEXT(3)
GLOBAL_UNCERTAINTY_ASSIGNED_CONTEXT((#33897))
GLOBAL_UNIT_ASSIGNED_CONTEXT((#33982,#33984,#33985))
REPRESENTATION_CONTEXT('','3D')
);
#33950=(
GEOMETRIC_REPRESENTATION_CONTEXT(3)
GLOBAL_UNCERTAINTY_ASSIGNED_CONTEXT((#33898))
GLOBAL_UNIT_ASSIGNED_CONTEXT((#33982,#33984,#33985))
REPRESENTATION_CONTEXT('','3D')
);
#33951=(
GEOMETRIC_REPRESENTATION_CONTEXT(3)
GLOBAL_UNCERTAINTY_ASSIGNED_CONTEXT((#33899))
GLOBAL_UNIT_ASSIGNED_CONTEXT((#33982,#33984,#33985))
REPRESENTATION_CONTEXT('','3D')
);
#33952=(
GEOMETRIC_REPRESENTATION_CONTEXT(3)
GLOBAL_UNCERTAINTY_ASSIGNED_CONTEXT((#33900))
GLOBAL_UNIT_ASSIGNED_CONTEXT((#33982,#33984,#33985))
REPRESENTATION_CONTEXT('','3D')
);
#33953=(
GEOMETRIC_REPRESENTATION_CONTEXT(3)
GLOBAL_UNCERTAINTY_ASSIGNED_CONTEXT((#33901))
GLOBAL_UNIT_ASSIGNED_CONTEXT((#33982,#33984,#33985))
REPRESENTATION_CONTEXT('','3D')
);
#33954=(
GEOMETRIC_REPRESENTATION_CONTEXT(3)
GLOBAL_UNCERTAINTY_ASSIGNED_CONTEXT((#33902))
GLOBAL_UNIT_ASSIGNED_CONTEXT((#33982,#33984,#33985))
REPRESENTATION_CONTEXT('','3D')
);
#33955=(
GEOMETRIC_REPRESENTATION_CONTEXT(3)
GLOBAL_UNCERTAINTY_ASSIGNED_CONTEXT((#33903))
GLOBAL_UNIT_ASSIGNED_CONTEXT((#33982,#33984,#33985))
REPRESENTATION_CONTEXT('','3D')
);
#33956=(
GEOMETRIC_REPRESENTATION_CONTEXT(3)
GLOBAL_UNCERTAINTY_ASSIGNED_CONTEXT((#33904))
GLOBAL_UNIT_ASSIGNED_CONTEXT((#33982,#33984,#33985))
REPRESENTATION_CONTEXT('','3D')
);
#33957=(
GEOMETRIC_REPRESENTATION_CONTEXT(3)
GLOBAL_UNCERTAINTY_ASSIGNED_CONTEXT((#33905))
GLOBAL_UNIT_ASSIGNED_CONTEXT((#33982,#33984,#33985))
REPRESENTATION_CONTEXT('','3D')
);
#33958=(
GEOMETRIC_REPRESENTATION_CONTEXT(3)
GLOBAL_UNCERTAINTY_ASSIGNED_CONTEXT((#33906))
GLOBAL_UNIT_ASSIGNED_CONTEXT((#33982,#33984,#33985))
REPRESENTATION_CONTEXT('','3D')
);
#33959=(
GEOMETRIC_REPRESENTATION_CONTEXT(3)
GLOBAL_UNCERTAINTY_ASSIGNED_CONTEXT((#33907))
GLOBAL_UNIT_ASSIGNED_CONTEXT((#33982,#33984,#33985))
REPRESENTATION_CONTEXT('','3D')
);
#33960=(
GEOMETRIC_REPRESENTATION_CONTEXT(3)
GLOBAL_UNCERTAINTY_ASSIGNED_CONTEXT((#33908))
GLOBAL_UNIT_ASSIGNED_CONTEXT((#33982,#33984,#33985))
REPRESENTATION_CONTEXT('','3D')
);
#33961=(
GEOMETRIC_REPRESENTATION_CONTEXT(3)
GLOBAL_UNCERTAINTY_ASSIGNED_CONTEXT((#33909))
GLOBAL_UNIT_ASSIGNED_CONTEXT((#33982,#33984,#33985))
REPRESENTATION_CONTEXT('','3D')
);
#33962=(
GEOMETRIC_REPRESENTATION_CONTEXT(3)
GLOBAL_UNCERTAINTY_ASSIGNED_CONTEXT((#33910))
GLOBAL_UNIT_ASSIGNED_CONTEXT((#33982,#33984,#33985))
REPRESENTATION_CONTEXT('','3D')
);
#33963=(
GEOMETRIC_REPRESENTATION_CONTEXT(3)
GLOBAL_UNCERTAINTY_ASSIGNED_CONTEXT((#33911))
GLOBAL_UNIT_ASSIGNED_CONTEXT((#33982,#33984,#33985))
REPRESENTATION_CONTEXT('','3D')
);
#33964=(
GEOMETRIC_REPRESENTATION_CONTEXT(3)
GLOBAL_UNCERTAINTY_ASSIGNED_CONTEXT((#33912))
GLOBAL_UNIT_ASSIGNED_CONTEXT((#33982,#33984,#33985))
REPRESENTATION_CONTEXT('','3D')
);
#33965=(
GEOMETRIC_REPRESENTATION_CONTEXT(3)
GLOBAL_UNCERTAINTY_ASSIGNED_CONTEXT((#33913))
GLOBAL_UNIT_ASSIGNED_CONTEXT((#33982,#33984,#33985))
REPRESENTATION_CONTEXT('','3D')
);
#33966=(
GEOMETRIC_REPRESENTATION_CONTEXT(3)
GLOBAL_UNCERTAINTY_ASSIGNED_CONTEXT((#33914))
GLOBAL_UNIT_ASSIGNED_CONTEXT((#33982,#33984,#33985))
REPRESENTATION_CONTEXT('','3D')
);
#33967=(
GEOMETRIC_REPRESENTATION_CONTEXT(3)
GLOBAL_UNCERTAINTY_ASSIGNED_CONTEXT((#33915))
GLOBAL_UNIT_ASSIGNED_CONTEXT((#33982,#33984,#33985))
REPRESENTATION_CONTEXT('','3D')
);
#33968=(
GEOMETRIC_REPRESENTATION_CONTEXT(3)
GLOBAL_UNCERTAINTY_ASSIGNED_CONTEXT((#33916))
GLOBAL_UNIT_ASSIGNED_CONTEXT((#33982,#33984,#33985))
REPRESENTATION_CONTEXT('','3D')
);
#33969=(
GEOMETRIC_REPRESENTATION_CONTEXT(3)
GLOBAL_UNCERTAINTY_ASSIGNED_CONTEXT((#33917))
GLOBAL_UNIT_ASSIGNED_CONTEXT((#33982,#33984,#33985))
REPRESENTATION_CONTEXT('','3D')
);
#33970=(
GEOMETRIC_REPRESENTATION_CONTEXT(3)
GLOBAL_UNCERTAINTY_ASSIGNED_CONTEXT((#33918))
GLOBAL_UNIT_ASSIGNED_CONTEXT((#33982,#33984,#33985))
REPRESENTATION_CONTEXT('','3D')
);
#33971=(
GEOMETRIC_REPRESENTATION_CONTEXT(3)
GLOBAL_UNCERTAINTY_ASSIGNED_CONTEXT((#33919))
GLOBAL_UNIT_ASSIGNED_CONTEXT((#33982,#33984,#33985))
REPRESENTATION_CONTEXT('','3D')
);
#33972=(
GEOMETRIC_REPRESENTATION_CONTEXT(3)
GLOBAL_UNCERTAINTY_ASSIGNED_CONTEXT((#33920))
GLOBAL_UNIT_ASSIGNED_CONTEXT((#33982,#33984,#33985))
REPRESENTATION_CONTEXT('','3D')
);
#33973=(
GEOMETRIC_REPRESENTATION_CONTEXT(3)
GLOBAL_UNCERTAINTY_ASSIGNED_CONTEXT((#33921))
GLOBAL_UNIT_ASSIGNED_CONTEXT((#33982,#33984,#33985))
REPRESENTATION_CONTEXT('','3D')
);
#33974=(
GEOMETRIC_REPRESENTATION_CONTEXT(3)
GLOBAL_UNCERTAINTY_ASSIGNED_CONTEXT((#33922))
GLOBAL_UNIT_ASSIGNED_CONTEXT((#33982,#33984,#33985))
REPRESENTATION_CONTEXT('','3D')
);
#33975=(
GEOMETRIC_REPRESENTATION_CONTEXT(3)
GLOBAL_UNCERTAINTY_ASSIGNED_CONTEXT((#33923))
GLOBAL_UNIT_ASSIGNED_CONTEXT((#33982,#33984,#33985))
REPRESENTATION_CONTEXT('','3D')
);
#33976=(
GEOMETRIC_REPRESENTATION_CONTEXT(3)
GLOBAL_UNCERTAINTY_ASSIGNED_CONTEXT((#33924))
GLOBAL_UNIT_ASSIGNED_CONTEXT((#33982,#33984,#33985))
REPRESENTATION_CONTEXT('','3D')
);
#33977=(
GEOMETRIC_REPRESENTATION_CONTEXT(3)
GLOBAL_UNCERTAINTY_ASSIGNED_CONTEXT((#33925))
GLOBAL_UNIT_ASSIGNED_CONTEXT((#33982,#33984,#33985))
REPRESENTATION_CONTEXT('','3D')
);
#33978=(
GEOMETRIC_REPRESENTATION_CONTEXT(3)
GLOBAL_UNCERTAINTY_ASSIGNED_CONTEXT((#33926))
GLOBAL_UNIT_ASSIGNED_CONTEXT((#33982,#33984,#33985))
REPRESENTATION_CONTEXT('','3D')
);
#33979=(
GEOMETRIC_REPRESENTATION_CONTEXT(3)
GLOBAL_UNCERTAINTY_ASSIGNED_CONTEXT((#33927))
GLOBAL_UNIT_ASSIGNED_CONTEXT((#33982,#33984,#33985))
REPRESENTATION_CONTEXT('','3D')
);
#33980=(
GEOMETRIC_REPRESENTATION_CONTEXT(3)
GLOBAL_UNCERTAINTY_ASSIGNED_CONTEXT((#33928))
GLOBAL_UNIT_ASSIGNED_CONTEXT((#33982,#33984,#33985))
REPRESENTATION_CONTEXT('','3D')
);
#33981=(
GEOMETRIC_REPRESENTATION_CONTEXT(3)
GLOBAL_UNCERTAINTY_ASSIGNED_CONTEXT((#33929))
GLOBAL_UNIT_ASSIGNED_CONTEXT((#33982,#33984,#33985))
REPRESENTATION_CONTEXT('','3D')
);
#33982=(
LENGTH_UNIT()
NAMED_UNIT(*)
SI_UNIT(.CENTI.,.METRE.)
);
#33983=(
LENGTH_UNIT()
NAMED_UNIT(*)
SI_UNIT($,.METRE.)
);
#33984=(
NAMED_UNIT(*)
PLANE_ANGLE_UNIT()
SI_UNIT($,.RADIAN.)
);
#33985=(
NAMED_UNIT(*)
SI_UNIT($,.STERADIAN.)
SOLID_ANGLE_UNIT()
);
#33986=SHAPE_DEFINITION_REPRESENTATION(#34037,#34182);
#33987=SHAPE_DEFINITION_REPRESENTATION(#34038,#34183);
#33988=SHAPE_DEFINITION_REPRESENTATION(#34039,#34184);
#33989=SHAPE_DEFINITION_REPRESENTATION(#34040,#34185);
#33990=SHAPE_DEFINITION_REPRESENTATION(#34041,#34186);
#33991=SHAPE_DEFINITION_REPRESENTATION(#34042,#34187);
#33992=SHAPE_DEFINITION_REPRESENTATION(#34043,#34188);
#33993=SHAPE_DEFINITION_REPRESENTATION(#34044,#34189);
#33994=SHAPE_DEFINITION_REPRESENTATION(#34045,#34190);
#33995=SHAPE_DEFINITION_REPRESENTATION(#34046,#34191);
#33996=SHAPE_DEFINITION_REPRESENTATION(#34047,#34192);
#33997=SHAPE_DEFINITION_REPRESENTATION(#34048,#34193);
#33998=SHAPE_DEFINITION_REPRESENTATION(#34049,#34194);
#33999=SHAPE_DEFINITION_REPRESENTATION(#34050,#34195);
#34000=SHAPE_DEFINITION_REPRESENTATION(#34051,#34196);
#34001=SHAPE_DEFINITION_REPRESENTATION(#34052,#34197);
#34002=SHAPE_DEFINITION_REPRESENTATION(#34053,#34198);
#34003=SHAPE_DEFINITION_REPRESENTATION(#34059,#34199);
#34004=SHAPE_DEFINITION_REPRESENTATION(#34060,#34200);
#34005=SHAPE_DEFINITION_REPRESENTATION(#34061,#34201);
#34006=SHAPE_DEFINITION_REPRESENTATION(#34062,#34202);
#34007=SHAPE_DEFINITION_REPRESENTATION(#34063,#34203);
#34008=SHAPE_DEFINITION_REPRESENTATION(#34064,#34204);
#34009=SHAPE_DEFINITION_REPRESENTATION(#34070,#34205);
#34010=SHAPE_DEFINITION_REPRESENTATION(#34071,#34206);
#34011=SHAPE_DEFINITION_REPRESENTATION(#34072,#34207);
#34012=SHAPE_DEFINITION_REPRESENTATION(#34073,#34208);
#34013=SHAPE_DEFINITION_REPRESENTATION(#34074,#34209);
#34014=SHAPE_DEFINITION_REPRESENTATION(#34075,#34210);
#34015=SHAPE_DEFINITION_REPRESENTATION(#34076,#34211);
#34016=SHAPE_DEFINITION_REPRESENTATION(#34077,#34212);
#34017=SHAPE_DEFINITION_REPRESENTATION(#34078,#34213);
#34018=SHAPE_DEFINITION_REPRESENTATION(#34079,#34214);
#34019=SHAPE_DEFINITION_REPRESENTATION(#34080,#34215);
#34020=SHAPE_DEFINITION_REPRESENTATION(#34081,#34216);
#34021=SHAPE_DEFINITION_REPRESENTATION(#34085,#34217);
#34022=SHAPE_DEFINITION_REPRESENTATION(#34086,#34218);
#34023=SHAPE_DEFINITION_REPRESENTATION(#34087,#34219);
#34024=SHAPE_DEFINITION_REPRESENTATION(#34088,#34220);
#34025=SHAPE_DEFINITION_REPRESENTATION(#34089,#34221);
#34026=SHAPE_DEFINITION_REPRESENTATION(#34110,#34222);
#34027=SHAPE_DEFINITION_REPRESENTATION(#34111,#34223);
#34028=SHAPE_DEFINITION_REPRESENTATION(#34112,#34224);
#34029=SHAPE_DEFINITION_REPRESENTATION(#34113,#34225);
#34030=SHAPE_DEFINITION_REPRESENTATION(#34114,#34226);
#34031=SHAPE_DEFINITION_REPRESENTATION(#34115,#34227);
#34032=SHAPE_DEFINITION_REPRESENTATION(#34116,#34228);
#34033=SHAPE_DEFINITION_REPRESENTATION(#34117,#34229);
#34034=SHAPE_DEFINITION_REPRESENTATION(#34118,#34230);
#34035=SHAPE_DEFINITION_REPRESENTATION(#34119,#34231);
#34036=SHAPE_DEFINITION_REPRESENTATION(#34120,#34232);
#34037=PRODUCT_DEFINITION_SHAPE('',$,#34234);
#34038=PRODUCT_DEFINITION_SHAPE('',$,#34235);
#34039=PRODUCT_DEFINITION_SHAPE('',$,#34236);
#34040=PRODUCT_DEFINITION_SHAPE('',$,#34237);
#34041=PRODUCT_DEFINITION_SHAPE('',$,#34238);
#34042=PRODUCT_DEFINITION_SHAPE('',$,#34239);
#34043=PRODUCT_DEFINITION_SHAPE('',$,#34240);
#34044=PRODUCT_DEFINITION_SHAPE('',$,#34241);
#34045=PRODUCT_DEFINITION_SHAPE('',$,#34242);
#34046=PRODUCT_DEFINITION_SHAPE('',$,#34243);
#34047=PRODUCT_DEFINITION_SHAPE('',$,#34244);
#34048=PRODUCT_DEFINITION_SHAPE('',$,#34245);
#34049=PRODUCT_DEFINITION_SHAPE('',$,#34246);
#34050=PRODUCT_DEFINITION_SHAPE('',$,#34247);
#34051=PRODUCT_DEFINITION_SHAPE('',$,#34248);
#34052=PRODUCT_DEFINITION_SHAPE('',$,#34249);
#34053=PRODUCT_DEFINITION_SHAPE('',$,#34250);
#34054=PRODUCT_DEFINITION_SHAPE($,$,#309);
#34055=PRODUCT_DEFINITION_SHAPE($,$,#310);
#34056=PRODUCT_DEFINITION_SHAPE($,$,#311);
#34057=PRODUCT_DEFINITION_SHAPE($,$,#312);
#34058=PRODUCT_DEFINITION_SHAPE($,$,#313);
#34059=PRODUCT_DEFINITION_SHAPE('',$,#34251);
#34060=PRODUCT_DEFINITION_SHAPE('',$,#34252);
#34061=PRODUCT_DEFINITION_SHAPE('',$,#34253);
#34062=PRODUCT_DEFINITION_SHAPE('',$,#34254);
#34063=PRODUCT_DEFINITION_SHAPE('',$,#34255);
#34064=PRODUCT_DEFINITION_SHAPE('',$,#34256);
#34065=PRODUCT_DEFINITION_SHAPE($,$,#314);
#34066=PRODUCT_DEFINITION_SHAPE($,$,#315);
#34067=PRODUCT_DEFINITION_SHAPE($,$,#316);
#34068=PRODUCT_DEFINITION_SHAPE($,$,#317);
#34069=PRODUCT_DEFINITION_SHAPE($,$,#318);
#34070=PRODUCT_DEFINITION_SHAPE('',$,#34257);
#34071=PRODUCT_DEFINITION_SHAPE('',$,#34258);
#34072=PRODUCT_DEFINITION_SHAPE('',$,#34259);
#34073=PRODUCT_DEFINITION_SHAPE('',$,#34260);
#34074=PRODUCT_DEFINITION_SHAPE('',$,#34261);
#34075=PRODUCT_DEFINITION_SHAPE('',$,#34262);
#34076=PRODUCT_DEFINITION_SHAPE('',$,#34263);
#34077=PRODUCT_DEFINITION_SHAPE('',$,#34264);
#34078=PRODUCT_DEFINITION_SHAPE('',$,#34265);
#34079=PRODUCT_DEFINITION_SHAPE('',$,#34266);
#34080=PRODUCT_DEFINITION_SHAPE('',$,#34267);
#34081=PRODUCT_DEFINITION_SHAPE('',$,#34268);
#34082=PRODUCT_DEFINITION_SHAPE($,$,#319);
#34083=PRODUCT_DEFINITION_SHAPE($,$,#320);
#34084=PRODUCT_DEFINITION_SHAPE($,$,#321);
#34085=PRODUCT_DEFINITION_SHAPE('',$,#34269);
#34086=PRODUCT_DEFINITION_SHAPE('',$,#34270);
#34087=PRODUCT_DEFINITION_SHAPE('',$,#34271);
#34088=PRODUCT_DEFINITION_SHAPE('',$,#34272);
#34089=PRODUCT_DEFINITION_SHAPE('',$,#34273);
#34090=PRODUCT_DEFINITION_SHAPE($,$,#322);
#34091=PRODUCT_DEFINITION_SHAPE($,$,#323);
#34092=PRODUCT_DEFINITION_SHAPE($,$,#324);
#34093=PRODUCT_DEFINITION_SHAPE($,$,#325);
#34094=PRODUCT_DEFINITION_SHAPE($,$,#326);
#34095=PRODUCT_DEFINITION_SHAPE($,$,#327);
#34096=PRODUCT_DEFINITION_SHAPE($,$,#328);
#34097=PRODUCT_DEFINITION_SHAPE($,$,#329);
#34098=PRODUCT_DEFINITION_SHAPE($,$,#330);
#34099=PRODUCT_DEFINITION_SHAPE($,$,#331);
#34100=PRODUCT_DEFINITION_SHAPE($,$,#332);
#34101=PRODUCT_DEFINITION_SHAPE($,$,#333);
#34102=PRODUCT_DEFINITION_SHAPE($,$,#334);
#34103=PRODUCT_DEFINITION_SHAPE($,$,#335);
#34104=PRODUCT_DEFINITION_SHAPE($,$,#336);
#34105=PRODUCT_DEFINITION_SHAPE($,$,#337);
#34106=PRODUCT_DEFINITION_SHAPE($,$,#338);
#34107=PRODUCT_DEFINITION_SHAPE($,$,#339);
#34108=PRODUCT_DEFINITION_SHAPE($,$,#340);
#34109=PRODUCT_DEFINITION_SHAPE($,$,#341);
#34110=PRODUCT_DEFINITION_SHAPE('',$,#34274);
#34111=PRODUCT_DEFINITION_SHAPE('',$,#34275);
#34112=PRODUCT_DEFINITION_SHAPE('',$,#34276);
#34113=PRODUCT_DEFINITION_SHAPE('',$,#34277);
#34114=PRODUCT_DEFINITION_SHAPE('',$,#34278);
#34115=PRODUCT_DEFINITION_SHAPE('',$,#34279);
#34116=PRODUCT_DEFINITION_SHAPE('',$,#34280);
#34117=PRODUCT_DEFINITION_SHAPE('',$,#34281);
#34118=PRODUCT_DEFINITION_SHAPE('',$,#34282);
#34119=PRODUCT_DEFINITION_SHAPE('',$,#34283);
#34120=PRODUCT_DEFINITION_SHAPE('',$,#34284);
#34121=PRODUCT_DEFINITION_SHAPE($,$,#342);
#34122=PRODUCT_DEFINITION_SHAPE($,$,#343);
#34123=PRODUCT_DEFINITION_SHAPE($,$,#344);
#34124=PRODUCT_DEFINITION_SHAPE($,$,#345);
#34125=PRODUCT_DEFINITION_SHAPE($,$,#346);
#34126=PRODUCT_DEFINITION_SHAPE($,$,#347);
#34127=PRODUCT_DEFINITION_SHAPE($,$,#348);
#34128=PRODUCT_DEFINITION_SHAPE($,$,#349);
#34129=PRODUCT_DEFINITION_SHAPE($,$,#350);
#34130=PRODUCT_DEFINITION_SHAPE($,$,#351);
#34131=PRODUCT_DEFINITION_SHAPE($,$,#352);
#34132=PRODUCT_DEFINITION_SHAPE($,$,#353);
#34133=PRODUCT_DEFINITION_SHAPE($,$,#354);
#34134=PRODUCT_DEFINITION_SHAPE($,$,#355);
#34135=PRODUCT_DEFINITION_SHAPE($,$,#356);
#34136=PRODUCT_DEFINITION_SHAPE($,$,#357);
#34137=PRODUCT_DEFINITION_SHAPE($,$,#358);
#34138=PRODUCT_DEFINITION_SHAPE($,$,#359);
#34139=PRODUCT_DEFINITION_SHAPE($,$,#360);
#34140=PRODUCT_DEFINITION_SHAPE($,$,#361);
#34141=PRODUCT_DEFINITION_SHAPE($,$,#362);
#34142=PRODUCT_DEFINITION_SHAPE($,$,#363);
#34143=PRODUCT_DEFINITION_SHAPE($,$,#364);
#34144=PRODUCT_DEFINITION_SHAPE($,$,#365);
#34145=PRODUCT_DEFINITION_SHAPE($,$,#366);
#34146=PRODUCT_DEFINITION_SHAPE($,$,#367);
#34147=PRODUCT_DEFINITION_SHAPE($,$,#368);
#34148=PRODUCT_DEFINITION_SHAPE($,$,#369);
#34149=PRODUCT_DEFINITION_SHAPE($,$,#370);
#34150=PRODUCT_DEFINITION_SHAPE($,$,#371);
#34151=PRODUCT_DEFINITION_SHAPE($,$,#372);
#34152=PRODUCT_DEFINITION_SHAPE($,$,#373);
#34153=PRODUCT_DEFINITION_SHAPE($,$,#374);
#34154=PRODUCT_DEFINITION_SHAPE($,$,#375);
#34155=PRODUCT_DEFINITION_SHAPE($,$,#376);
#34156=PRODUCT_DEFINITION_SHAPE($,$,#377);
#34157=PRODUCT_DEFINITION_SHAPE($,$,#378);
#34158=PRODUCT_DEFINITION_SHAPE($,$,#379);
#34159=PRODUCT_DEFINITION_SHAPE($,$,#380);
#34160=PRODUCT_DEFINITION_SHAPE($,$,#381);
#34161=PRODUCT_DEFINITION_SHAPE($,$,#382);
#34162=PRODUCT_DEFINITION_SHAPE($,$,#383);
#34163=PRODUCT_DEFINITION_SHAPE($,$,#384);
#34164=PRODUCT_DEFINITION_SHAPE($,$,#385);
#34165=PRODUCT_DEFINITION_SHAPE($,$,#386);
#34166=PRODUCT_DEFINITION_SHAPE($,$,#387);
#34167=PRODUCT_DEFINITION_SHAPE($,$,#388);
#34168=PRODUCT_DEFINITION_SHAPE($,$,#389);
#34169=PRODUCT_DEFINITION_SHAPE($,$,#390);
#34170=PRODUCT_DEFINITION_SHAPE($,$,#391);
#34171=PRODUCT_DEFINITION_SHAPE($,$,#392);
#34172=PRODUCT_DEFINITION_SHAPE($,$,#393);
#34173=PRODUCT_DEFINITION_SHAPE($,$,#394);
#34174=PRODUCT_DEFINITION_SHAPE($,$,#395);
#34175=PRODUCT_DEFINITION_SHAPE($,$,#396);
#34176=PRODUCT_DEFINITION_SHAPE($,$,#397);
#34177=PRODUCT_DEFINITION_SHAPE($,$,#398);
#34178=PRODUCT_DEFINITION_SHAPE($,$,#399);
#34179=PRODUCT_DEFINITION_SHAPE($,$,#400);
#34180=PRODUCT_DEFINITION_SHAPE($,$,#401);
#34181=PRODUCT_DEFINITION_SHAPE($,$,#402);
#34182=SHAPE_REPRESENTATION('',(#13559,#14887,#14888,#14889),#33930);
#34183=SHAPE_REPRESENTATION('',(#13560,#14829,#14830,#14831,#14832,#14833,
#14834,#14835,#14836,#14837,#14838,#14839,#14840,#14841,#14842,#14843,#14844,
#14845,#14846,#14847,#14848,#14849,#14850,#14851,#14852,#14853,#14854,#14855,
#14856,#14857,#14858,#14859,#14860,#14861,#14862,#14863,#14864,#14865,#14866,
#14867,#14868,#14869,#14870,#14871,#14872,#14873,#14874,#14875),#33931);
#34184=SHAPE_REPRESENTATION('',(#13561),#33932);
#34185=SHAPE_REPRESENTATION('',(#13616),#33933);
#34186=SHAPE_REPRESENTATION('',(#13663),#33934);
#34187=SHAPE_REPRESENTATION('',(#13694),#33935);
#34188=SHAPE_REPRESENTATION('',(#13716),#33936);
#34189=SHAPE_REPRESENTATION('',(#13747),#33937);
#34190=SHAPE_REPRESENTATION('',(#13770),#33938);
#34191=SHAPE_REPRESENTATION('',(#13799),#33939);
#34192=SHAPE_REPRESENTATION('',(#13828),#33940);
#34193=SHAPE_REPRESENTATION('',(#13871,#13994,#13995,#13996,#13997,#13998),
#33941);
#34194=SHAPE_REPRESENTATION('',(#13872),#33942);
#34195=SHAPE_REPRESENTATION('',(#13892),#33943);
#34196=SHAPE_REPRESENTATION('',(#13912),#33944);
#34197=SHAPE_REPRESENTATION('',(#13927),#33945);
#34198=SHAPE_REPRESENTATION('',(#13977),#33946);
#34199=SHAPE_REPRESENTATION('',(#13999,#14128,#14129,#14130,#14131,#14132),
#33947);
#34200=SHAPE_REPRESENTATION('',(#14000),#33948);
#34201=SHAPE_REPRESENTATION('',(#14020),#33949);
#34202=SHAPE_REPRESENTATION('',(#14040),#33950);
#34203=SHAPE_REPRESENTATION('',(#14057),#33951);
#34204=SHAPE_REPRESENTATION('',(#14111),#33952);
#34205=SHAPE_REPRESENTATION('',(#14133),#33953);
#34206=SHAPE_REPRESENTATION('',(#14183),#33954);
#34207=SHAPE_REPRESENTATION('',(#14200),#33955);
#34208=SHAPE_REPRESENTATION('',(#14211),#33956);
#34209=SHAPE_REPRESENTATION('',(#14235,#14525,#14526,#14527,#14528,#14529,
#14530,#14531,#14532,#14533,#14534,#14535,#14536,#14537,#14538,#14539,#14540,
#14541,#14542,#14543,#14544),#33957);
#34210=SHAPE_REPRESENTATION('',(#14236),#33958);
#34211=SHAPE_REPRESENTATION('',(#14255),#33959);
#34212=SHAPE_REPRESENTATION('',(#14286),#33960);
#34213=SHAPE_REPRESENTATION('',(#14324,#14386,#14387,#14388),#33961);
#34214=SHAPE_REPRESENTATION('',(#14325),#33962);
#34215=SHAPE_REPRESENTATION('',(#14364),#33963);
#34216=SHAPE_REPRESENTATION('',(#14375),#33964);
#34217=SHAPE_REPRESENTATION('',(#14389),#33965);
#34218=SHAPE_REPRESENTATION('',(#14400),#33966);
#34219=SHAPE_REPRESENTATION('',(#14428),#33967);
#34220=SHAPE_REPRESENTATION('',(#14473),#33968);
#34221=SHAPE_REPRESENTATION('',(#14499),#33969);
#34222=SHAPE_REPRESENTATION('',(#14545,#14876,#14877,#14878,#14879,#14880,
#14881,#14882,#14883,#14884,#14885,#14886),#33970);
#34223=SHAPE_REPRESENTATION('',(#14546),#33971);
#34224=SHAPE_REPRESENTATION('',(#14701),#33972);
#34225=SHAPE_REPRESENTATION('',(#14710),#33973);
#34226=SHAPE_REPRESENTATION('',(#14724),#33974);
#34227=SHAPE_REPRESENTATION('',(#14748),#33975);
#34228=SHAPE_REPRESENTATION('',(#14757),#33976);
#34229=SHAPE_REPRESENTATION('',(#14766),#33977);
#34230=SHAPE_REPRESENTATION('',(#14777),#33978);
#34231=SHAPE_REPRESENTATION('',(#14794),#33979);
#34232=SHAPE_REPRESENTATION('',(#14803),#33980);
#34233=PRODUCT_DEFINITION_CONTEXT('part definition',#34388,'design');
#34234=PRODUCT_DEFINITION('PAT-054',
'PAT-054',#34285,#34233);
#34235=PRODUCT_DEFINITION('Rail and screw supports',
'Rail and screw supports',#34286,#34233);
#34236=PRODUCT_DEFINITION('Runner-mounted base','Runner-mounted base',#34287,
#34233);
#34237=PRODUCT_DEFINITION('Rail adapter','Rail adapter',#34288,#34233);
#34238=PRODUCT_DEFINITION('Floating bearing support',
'Floating bearing support',#34289,#34233);
#34239=PRODUCT_DEFINITION('Floating cap','Floating cap',#34290,#34233);
#34240=PRODUCT_DEFINITION('Fixed bearing support',
'Fixed bearing support',#34291,#34233);
#34241=PRODUCT_DEFINITION('Fixed cap','Fixed cap',#34292,#34233);
#34242=PRODUCT_DEFINITION('End stop','End stop',#34293,#34233);
#34243=PRODUCT_DEFINITION('End stop (1)','End stop (1)',#34294,#34233);
#34244=PRODUCT_DEFINITION('Linear Guide Rail - 15 mm, 220 mm Long',
'Linear Guide Rail - 15 mm, 220 mm Long',#34295,#34233);
#34245=PRODUCT_DEFINITION('Sealed Ball Bearing - 12 x 32 x 10 mm',
'Sealed Ball Bearing - 12 x 32 x 10 mm',#34296,#34233);
#34246=PRODUCT_DEFINITION('Inner ring','Inner ring',#34297,#34233);
#34247=PRODUCT_DEFINITION('Outer ring','Outer ring',#34298,#34233);
#34248=PRODUCT_DEFINITION('Balls','Balls',#34299,#34233);
#34249=PRODUCT_DEFINITION('Cage','Cage',#34300,#34233);
#34250=PRODUCT_DEFINITION('Seals 2RS','Seals 2RS',#34301,#34233);
#34251=PRODUCT_DEFINITION('Sealed Ball Bearing - 20 x 47 x 14 mm',
'Sealed Ball Bearing - 20 x 47 x 14 mm',#34302,#34233);
#34252=PRODUCT_DEFINITION('Inner ring (1)','Inner ring (1)',#34303,#34233);
#34253=PRODUCT_DEFINITION('Outer ring (1)','Outer ring (1)',#34304,#34233);
#34254=PRODUCT_DEFINITION('Balls (1)','Balls (1)',#34305,#34233);
#34255=PRODUCT_DEFINITION('Cage (1)','Cage (1)',#34306,#34233);
#34256=PRODUCT_DEFINITION('Seals 2RS (1)','Seals 2RS (1)',#34307,#34233);
#34257=PRODUCT_DEFINITION('Slotted Extrusion - 20 x 20 x 300 mm',
'Slotted Extrusion - 20 x 20 x 300 mm',#34308,#34233);
#34258=PRODUCT_DEFINITION('Slot Nut - M5 for 20 mm Extrusion',
'Slot Nut - M5 for 20 mm Extrusion',#34309,#34233);
#34259=PRODUCT_DEFINITION('Flat Washer - M5','Flat Washer - M5',#34310,
#34233);
#34260=PRODUCT_DEFINITION('M5x18 runner screw','M5x18 runner screw',#34311,
#34233);
#34261=PRODUCT_DEFINITION('Moving table and nut','Moving table and nut',
#34312,#34233);
#34262=PRODUCT_DEFINITION('Carriage spacer','Carriage spacer',#34313,#34233);
#34263=PRODUCT_DEFINITION('Table','Table',#34314,#34233);
#34264=PRODUCT_DEFINITION('Nut bracket','Nut bracket',#34315,#34233);
#34265=PRODUCT_DEFINITION('Flanged Linear Guide Carriage - 15 mm',
'Flanged Linear Guide Carriage - 15 mm',#34316,#34233);
#34266=PRODUCT_DEFINITION('Block','Block',#34317,#34233);
#34267=PRODUCT_DEFINITION('End cap +','End cap +',#34318,#34233);
#34268=PRODUCT_DEFINITION('End cap','End cap',#34319,#34233);
#34269=PRODUCT_DEFINITION('Flat Washer - M5 (1)','Flat Washer - M5 (1)',#34320,
#34233);
#34270=PRODUCT_DEFINITION('M5x30 frame screw','M5x30 frame screw',#34321,
#34233);
#34271=PRODUCT_DEFINITION('Flanged lead nut','Flanged lead nut',#34322,
#34233);
#34272=PRODUCT_DEFINITION('Cap Screw - M4x16','Cap Screw - M4x16',#34323,
#34233);
#34273=PRODUCT_DEFINITION('Cap Screw - M5x20','Cap Screw - M5x20',#34324,
#34233);
#34274=PRODUCT_DEFINITION('Lead screw and handwheel',
'Lead screw and handwheel',#34325,#34233);
#34275=PRODUCT_DEFINITION('Supported TR12x3 screw',
'Supported TR12x3 screw',#34326,#34233);
#34276=PRODUCT_DEFINITION('Inner race spacer','Inner race spacer',#34327,
#34233);
#34277=PRODUCT_DEFINITION('Shaft retaining collar',
'Shaft retaining collar',#34328,#34233);
#34278=PRODUCT_DEFINITION('Handwheel','Handwheel',#34329,#34233);
#34279=PRODUCT_DEFINITION('Handle pivot sleeve','Handle pivot sleeve',#34330,
#34233);
#34280=PRODUCT_DEFINITION('Revolving handle','Revolving handle',#34331,
#34233);
#34281=PRODUCT_DEFINITION('Key 6x6x20','Key 6x6x20',#34332,#34233);
#34282=PRODUCT_DEFINITION('Socket Set Screw - M5x8',
'Socket Set Screw - M5x8',#34333,#34233);
#34283=PRODUCT_DEFINITION('Flat Washer - M6','Flat Washer - M6',#34334,
#34233);
#34284=PRODUCT_DEFINITION('Cap Screw - M6x25','Cap Screw - M6x25',#34335,
#34233);
#34285=PRODUCT_DEFINITION_FORMATION('',$,#34390);
#34286=PRODUCT_DEFINITION_FORMATION('',$,#34391);
#34287=PRODUCT_DEFINITION_FORMATION('',$,#34392);
#34288=PRODUCT_DEFINITION_FORMATION('',$,#34393);
#34289=PRODUCT_DEFINITION_FORMATION('',$,#34394);
#34290=PRODUCT_DEFINITION_FORMATION('',$,#34395);
#34291=PRODUCT_DEFINITION_FORMATION('',$,#34396);
#34292=PRODUCT_DEFINITION_FORMATION('',$,#34397);
#34293=PRODUCT_DEFINITION_FORMATION('',$,#34398);
#34294=PRODUCT_DEFINITION_FORMATION('',$,#34399);
#34295=PRODUCT_DEFINITION_FORMATION('',$,#34400);
#34296=PRODUCT_DEFINITION_FORMATION('',$,#34401);
#34297=PRODUCT_DEFINITION_FORMATION('',$,#34402);
#34298=PRODUCT_DEFINITION_FORMATION('',$,#34403);
#34299=PRODUCT_DEFINITION_FORMATION('',$,#34404);
#34300=PRODUCT_DEFINITION_FORMATION('',$,#34405);
#34301=PRODUCT_DEFINITION_FORMATION('',$,#34406);
#34302=PRODUCT_DEFINITION_FORMATION('',$,#34407);
#34303=PRODUCT_DEFINITION_FORMATION('',$,#34408);
#34304=PRODUCT_DEFINITION_FORMATION('',$,#34409);
#34305=PRODUCT_DEFINITION_FORMATION('',$,#34410);
#34306=PRODUCT_DEFINITION_FORMATION('',$,#34411);
#34307=PRODUCT_DEFINITION_FORMATION('',$,#34412);
#34308=PRODUCT_DEFINITION_FORMATION('',$,#34413);
#34309=PRODUCT_DEFINITION_FORMATION('',$,#34414);
#34310=PRODUCT_DEFINITION_FORMATION('',$,#34415);
#34311=PRODUCT_DEFINITION_FORMATION('',$,#34416);
#34312=PRODUCT_DEFINITION_FORMATION('',$,#34417);
#34313=PRODUCT_DEFINITION_FORMATION('',$,#34418);
#34314=PRODUCT_DEFINITION_FORMATION('',$,#34419);
#34315=PRODUCT_DEFINITION_FORMATION('',$,#34420);
#34316=PRODUCT_DEFINITION_FORMATION('',$,#34421);
#34317=PRODUCT_DEFINITION_FORMATION('',$,#34422);
#34318=PRODUCT_DEFINITION_FORMATION('',$,#34423);
#34319=PRODUCT_DEFINITION_FORMATION('',$,#34424);
#34320=PRODUCT_DEFINITION_FORMATION('',$,#34425);
#34321=PRODUCT_DEFINITION_FORMATION('',$,#34426);
#34322=PRODUCT_DEFINITION_FORMATION('',$,#34427);
#34323=PRODUCT_DEFINITION_FORMATION('',$,#34428);
#34324=PRODUCT_DEFINITION_FORMATION('',$,#34429);
#34325=PRODUCT_DEFINITION_FORMATION('',$,#34430);
#34326=PRODUCT_DEFINITION_FORMATION('',$,#34431);
#34327=PRODUCT_DEFINITION_FORMATION('',$,#34432);
#34328=PRODUCT_DEFINITION_FORMATION('',$,#34433);
#34329=PRODUCT_DEFINITION_FORMATION('',$,#34434);
#34330=PRODUCT_DEFINITION_FORMATION('',$,#34435);
#34331=PRODUCT_DEFINITION_FORMATION('',$,#34436);
#34332=PRODUCT_DEFINITION_FORMATION('',$,#34437);
#34333=PRODUCT_DEFINITION_FORMATION('',$,#34438);
#34334=PRODUCT_DEFINITION_FORMATION('',$,#34439);
#34335=PRODUCT_DEFINITION_FORMATION('',$,#34440);
#34336=PRODUCT_RELATED_PRODUCT_CATEGORY('PAT-054',
'PAT-054',(#34390));
#34337=PRODUCT_RELATED_PRODUCT_CATEGORY('Rail and screw supports',
'Rail and screw supports',(#34391));
#34338=PRODUCT_RELATED_PRODUCT_CATEGORY('Runner-mounted base',
'Runner-mounted base',(#34392));
#34339=PRODUCT_RELATED_PRODUCT_CATEGORY('Rail adapter','Rail adapter',(#34393));
#34340=PRODUCT_RELATED_PRODUCT_CATEGORY('Floating bearing support',
'Floating bearing support',(#34394));
#34341=PRODUCT_RELATED_PRODUCT_CATEGORY('Floating cap','Floating cap',(#34395));
#34342=PRODUCT_RELATED_PRODUCT_CATEGORY('Fixed bearing support',
'Fixed bearing support',(#34396));
#34343=PRODUCT_RELATED_PRODUCT_CATEGORY('Fixed cap','Fixed cap',(#34397));
#34344=PRODUCT_RELATED_PRODUCT_CATEGORY('End stop','End stop',(#34398));
#34345=PRODUCT_RELATED_PRODUCT_CATEGORY('End stop (1)','End stop (1)',(#34399));
#34346=PRODUCT_RELATED_PRODUCT_CATEGORY(
'Linear Guide Rail - 15 mm, 220 mm Long',
'Linear Guide Rail - 15 mm, 220 mm Long',(#34400));
#34347=PRODUCT_RELATED_PRODUCT_CATEGORY(
'Sealed Ball Bearing - 12 x 32 x 10 mm',
'Sealed Ball Bearing - 12 x 32 x 10 mm',(#34401));
#34348=PRODUCT_RELATED_PRODUCT_CATEGORY('Inner ring','Inner ring',(#34402));
#34349=PRODUCT_RELATED_PRODUCT_CATEGORY('Outer ring','Outer ring',(#34403));
#34350=PRODUCT_RELATED_PRODUCT_CATEGORY('Balls','Balls',(#34404));
#34351=PRODUCT_RELATED_PRODUCT_CATEGORY('Cage','Cage',(#34405));
#34352=PRODUCT_RELATED_PRODUCT_CATEGORY('Seals 2RS','Seals 2RS',(#34406));
#34353=PRODUCT_RELATED_PRODUCT_CATEGORY(
'Sealed Ball Bearing - 20 x 47 x 14 mm',
'Sealed Ball Bearing - 20 x 47 x 14 mm',(#34407));
#34354=PRODUCT_RELATED_PRODUCT_CATEGORY('Inner ring (1)',
'Inner ring (1)',(#34408));
#34355=PRODUCT_RELATED_PRODUCT_CATEGORY('Outer ring (1)',
'Outer ring (1)',(#34409));
#34356=PRODUCT_RELATED_PRODUCT_CATEGORY('Balls (1)','Balls (1)',(#34410));
#34357=PRODUCT_RELATED_PRODUCT_CATEGORY('Cage (1)','Cage (1)',(#34411));
#34358=PRODUCT_RELATED_PRODUCT_CATEGORY('Seals 2RS (1)','Seals 2RS (1)',
(#34412));
#34359=PRODUCT_RELATED_PRODUCT_CATEGORY(
'Slotted Extrusion - 20 x 20 x 300 mm',
'Slotted Extrusion - 20 x 20 x 300 mm',(#34413));
#34360=PRODUCT_RELATED_PRODUCT_CATEGORY(
'Slot Nut - M5 for 20 mm Extrusion','Slot Nut - M5 for 20 mm Extrusion',
(#34414));
#34361=PRODUCT_RELATED_PRODUCT_CATEGORY('Flat Washer - M5',
'Flat Washer - M5',(#34415));
#34362=PRODUCT_RELATED_PRODUCT_CATEGORY('M5x18 runner screw',
'M5x18 runner screw',(#34416));
#34363=PRODUCT_RELATED_PRODUCT_CATEGORY('Moving table and nut',
'Moving table and nut',(#34417));
#34364=PRODUCT_RELATED_PRODUCT_CATEGORY('Carriage spacer',
'Carriage spacer',(#34418));
#34365=PRODUCT_RELATED_PRODUCT_CATEGORY('Table','Table',(#34419));
#34366=PRODUCT_RELATED_PRODUCT_CATEGORY('Nut bracket','Nut bracket',(#34420));
#34367=PRODUCT_RELATED_PRODUCT_CATEGORY(
'Flanged Linear Guide Carriage - 15 mm',
'Flanged Linear Guide Carriage - 15 mm',(#34421));
#34368=PRODUCT_RELATED_PRODUCT_CATEGORY('Block','Block',(#34422));
#34369=PRODUCT_RELATED_PRODUCT_CATEGORY('End cap +','End cap +',(#34423));
#34370=PRODUCT_RELATED_PRODUCT_CATEGORY('End cap','End cap',(#34424));
#34371=PRODUCT_RELATED_PRODUCT_CATEGORY('Flat Washer - M5 (1)',
'Flat Washer - M5 (1)',(#34425));
#34372=PRODUCT_RELATED_PRODUCT_CATEGORY('M5x30 frame screw',
'M5x30 frame screw',(#34426));
#34373=PRODUCT_RELATED_PRODUCT_CATEGORY('Flanged lead nut',
'Flanged lead nut',(#34427));
#34374=PRODUCT_RELATED_PRODUCT_CATEGORY('Cap Screw - M4x16',
'Cap Screw - M4x16',(#34428));
#34375=PRODUCT_RELATED_PRODUCT_CATEGORY('Cap Screw - M5x20',
'Cap Screw - M5x20',(#34429));
#34376=PRODUCT_RELATED_PRODUCT_CATEGORY('Lead screw and handwheel',
'Lead screw and handwheel',(#34430));
#34377=PRODUCT_RELATED_PRODUCT_CATEGORY('Supported TR12x3 screw',
'Supported TR12x3 screw',(#34431));
#34378=PRODUCT_RELATED_PRODUCT_CATEGORY('Inner race spacer',
'Inner race spacer',(#34432));
#34379=PRODUCT_RELATED_PRODUCT_CATEGORY('Shaft retaining collar',
'Shaft retaining collar',(#34433));
#34380=PRODUCT_RELATED_PRODUCT_CATEGORY('Handwheel','Handwheel',(#34434));
#34381=PRODUCT_RELATED_PRODUCT_CATEGORY('Handle pivot sleeve',
'Handle pivot sleeve',(#34435));
#34382=PRODUCT_RELATED_PRODUCT_CATEGORY('Revolving handle',
'Revolving handle',(#34436));
#34383=PRODUCT_RELATED_PRODUCT_CATEGORY('Key 6x6x20','Key 6x6x20',(#34437));
#34384=PRODUCT_RELATED_PRODUCT_CATEGORY('Socket Set Screw - M5x8',
'Socket Set Screw - M5x8',(#34438));
#34385=PRODUCT_RELATED_PRODUCT_CATEGORY('Flat Washer - M6',
'Flat Washer - M6',(#34439));
#34386=PRODUCT_RELATED_PRODUCT_CATEGORY('Cap Screw - M6x25',
'Cap Screw - M6x25',(#34440));
#34387=APPLICATION_PROTOCOL_DEFINITION('international standard',
'automotive_design',2009,#34388);
#34388=APPLICATION_CONTEXT(
'Core Data for Automotive Mechanical Design Process');
#34389=PRODUCT_CONTEXT('part definition',#34388,'mechanical');
#34390=PRODUCT('PAT-054',
'PAT-054','PAT-054',(#34389));
#34391=PRODUCT('Rail and screw supports','Rail and screw supports',
'Rail and screw supports',(#34389));
#34392=PRODUCT('Runner-mounted base','Runner-mounted base',
'Runner-mounted base',(#34389));
#34393=PRODUCT('Rail adapter','Rail adapter','Rail adapter',(#34389));
#34394=PRODUCT('Floating bearing support','Floating bearing support',
'Floating bearing support',(#34389));
#34395=PRODUCT('Floating cap','Floating cap','Floating cap',(#34389));
#34396=PRODUCT('Fixed bearing support','Fixed bearing support',
'Fixed bearing support',(#34389));
#34397=PRODUCT('Fixed cap','Fixed cap','Fixed cap',(#34389));
#34398=PRODUCT('End stop','End stop','End stop',(#34389));
#34399=PRODUCT('End stop (1)','End stop (1)','End stop (1)',(#34389));
#34400=PRODUCT('Linear Guide Rail - 15 mm, 220 mm Long',
'Linear Guide Rail - 15 mm, 220 mm Long',
'Linear Guide Rail - 15 mm, 220 mm Long',(#34389));
#34401=PRODUCT('Sealed Ball Bearing - 12 x 32 x 10 mm',
'Sealed Ball Bearing - 12 x 32 x 10 mm',
'Sealed Ball Bearing - 12 x 32 x 10 mm',(#34389));
#34402=PRODUCT('Inner ring','Inner ring','Inner ring',(#34389));
#34403=PRODUCT('Outer ring','Outer ring','Outer ring',(#34389));
#34404=PRODUCT('Balls','Balls','Balls',(#34389));
#34405=PRODUCT('Cage','Cage','Cage',(#34389));
#34406=PRODUCT('Seals 2RS','Seals 2RS','Seals 2RS',(#34389));
#34407=PRODUCT('Sealed Ball Bearing - 20 x 47 x 14 mm',
'Sealed Ball Bearing - 20 x 47 x 14 mm',
'Sealed Ball Bearing - 20 x 47 x 14 mm',(#34389));
#34408=PRODUCT('Inner ring (1)','Inner ring (1)','Inner ring (1)',(#34389));
#34409=PRODUCT('Outer ring (1)','Outer ring (1)','Outer ring (1)',(#34389));
#34410=PRODUCT('Balls (1)','Balls (1)','Balls (1)',(#34389));
#34411=PRODUCT('Cage (1)','Cage (1)','Cage (1)',(#34389));
#34412=PRODUCT('Seals 2RS (1)','Seals 2RS (1)','Seals 2RS (1)',(#34389));
#34413=PRODUCT('Slotted Extrusion - 20 x 20 x 300 mm',
'Slotted Extrusion - 20 x 20 x 300 mm',
'Slotted Extrusion - 20 x 20 x 300 mm',(#34389));
#34414=PRODUCT('Slot Nut - M5 for 20 mm Extrusion',
'Slot Nut - M5 for 20 mm Extrusion','Slot Nut - M5 for 20 mm Extrusion',
(#34389));
#34415=PRODUCT('Flat Washer - M5','Flat Washer - M5','Flat Washer - M5',
(#34389));
#34416=PRODUCT('M5x18 runner screw','M5x18 runner screw',
'M5x18 runner screw',(#34389));
#34417=PRODUCT('Moving table and nut','Moving table and nut',
'Moving table and nut',(#34389));
#34418=PRODUCT('Carriage spacer','Carriage spacer','Carriage spacer',(#34389));
#34419=PRODUCT('Table','Table','Table',(#34389));
#34420=PRODUCT('Nut bracket','Nut bracket','Nut bracket',(#34389));
#34421=PRODUCT('Flanged Linear Guide Carriage - 15 mm',
'Flanged Linear Guide Carriage - 15 mm',
'Flanged Linear Guide Carriage - 15 mm',(#34389));
#34422=PRODUCT('Block','Block','Block',(#34389));
#34423=PRODUCT('End cap +','End cap +','End cap +',(#34389));
#34424=PRODUCT('End cap','End cap','End cap',(#34389));
#34425=PRODUCT('Flat Washer - M5 (1)','Flat Washer - M5 (1)',
'Flat Washer - M5 (1)',(#34389));
#34426=PRODUCT('M5x30 frame screw','M5x30 frame screw',
'M5x30 frame screw',(#34389));
#34427=PRODUCT('Flanged lead nut','Flanged lead nut','Flanged lead nut',
(#34389));
#34428=PRODUCT('Cap Screw - M4x16','Cap Screw - M4x16',
'Cap Screw - M4x16',(#34389));
#34429=PRODUCT('Cap Screw - M5x20','Cap Screw - M5x20',
'Cap Screw - M5x20',(#34389));
#34430=PRODUCT('Lead screw and handwheel','Lead screw and handwheel',
'Lead screw and handwheel',(#34389));
#34431=PRODUCT('Supported TR12x3 screw','Supported TR12x3 screw',
'Supported TR12x3 screw',(#34389));
#34432=PRODUCT('Inner race spacer','Inner race spacer',
'Inner race spacer',(#34389));
#34433=PRODUCT('Shaft retaining collar','Shaft retaining collar',
'Shaft retaining collar',(#34389));
#34434=PRODUCT('Handwheel','Handwheel','Handwheel',(#34389));
#34435=PRODUCT('Handle pivot sleeve','Handle pivot sleeve',
'Handle pivot sleeve',(#34389));
#34436=PRODUCT('Revolving handle','Revolving handle','Revolving handle',
(#34389));
#34437=PRODUCT('Key 6x6x20','Key 6x6x20','Key 6x6x20',(#34389));
#34438=PRODUCT('Socket Set Screw - M5x8','Socket Set Screw - M5x8',
'Socket Set Screw - M5x8',(#34389));
#34439=PRODUCT('Flat Washer - M6','Flat Washer - M6','Flat Washer - M6',
(#34389));
#34440=PRODUCT('Cap Screw - M6x25','Cap Screw - M6x25',
'Cap Screw - M6x25',(#34389));
#34441=PRESENTATION_STYLE_ASSIGNMENT((#34448));
#34442=PRESENTATION_STYLE_ASSIGNMENT((#34449));
#34443=PRESENTATION_STYLE_ASSIGNMENT((#34450));
#34444=PRESENTATION_STYLE_ASSIGNMENT((#34451));
#34445=PRESENTATION_STYLE_ASSIGNMENT((#34452));
#34446=PRESENTATION_STYLE_ASSIGNMENT((#34453));
#34447=PRESENTATION_STYLE_ASSIGNMENT((#34454));
#34448=SURFACE_STYLE_USAGE(.BOTH.,#34455);
#34449=SURFACE_STYLE_USAGE(.BOTH.,#34456);
#34450=SURFACE_STYLE_USAGE(.BOTH.,#34457);
#34451=SURFACE_STYLE_USAGE(.BOTH.,#34458);
#34452=SURFACE_STYLE_USAGE(.BOTH.,#34459);
#34453=SURFACE_STYLE_USAGE(.BOTH.,#34460);
#34454=SURFACE_STYLE_USAGE(.BOTH.,#34461);
#34455=SURFACE_SIDE_STYLE('',(#34462));
#34456=SURFACE_SIDE_STYLE('',(#34463));
#34457=SURFACE_SIDE_STYLE('',(#34464));
#34458=SURFACE_SIDE_STYLE('',(#34465));
#34459=SURFACE_SIDE_STYLE('',(#34466));
#34460=SURFACE_SIDE_STYLE('',(#34467));
#34461=SURFACE_SIDE_STYLE('',(#34468));
#34462=SURFACE_STYLE_FILL_AREA(#34469);
#34463=SURFACE_STYLE_FILL_AREA(#34470);
#34464=SURFACE_STYLE_FILL_AREA(#34471);
#34465=SURFACE_STYLE_FILL_AREA(#34472);
#34466=SURFACE_STYLE_FILL_AREA(#34473);
#34467=SURFACE_STYLE_FILL_AREA(#34474);
#34468=SURFACE_STYLE_FILL_AREA(#34475);
#34469=FILL_AREA_STYLE('Steel - Satin',(#34476));
#34470=FILL_AREA_STYLE('CAD Library Painted - Deep blue',(#34477));
#34471=FILL_AREA_STYLE('CAD Library Painted - Steel gray',(#34478));
#34472=FILL_AREA_STYLE('CAD Library Painted - Engineering blue',(#34479));
#34473=FILL_AREA_STYLE('CAD Library Painted - Off white',(#34480));
#34474=FILL_AREA_STYLE('CAD Library Painted - Graphite',(#34481));
#34475=FILL_AREA_STYLE('CAD Library Painted - Light blue',(#34482));
#34476=FILL_AREA_STYLE_COLOUR('Steel - Satin',#34483);
#34477=FILL_AREA_STYLE_COLOUR('CAD Library Painted - Deep blue',#34484);
#34478=FILL_AREA_STYLE_COLOUR('CAD Library Painted - Steel gray',#34485);
#34479=FILL_AREA_STYLE_COLOUR('CAD Library Painted - Engineering blue',
#34486);
#34480=FILL_AREA_STYLE_COLOUR('CAD Library Painted - Off white',#34487);
#34481=FILL_AREA_STYLE_COLOUR('CAD Library Painted - Graphite',#34488);
#34482=FILL_AREA_STYLE_COLOUR('CAD Library Painted - Light blue',#34489);
#34483=COLOUR_RGB('Steel - Satin',0.627450980392157,0.627450980392157,0.627450980392157);
#34484=COLOUR_RGB('CAD Library Painted - Deep blue',0.0784313725490196,
0.203921568627451,0.349019607843137);
#34485=COLOUR_RGB('CAD Library Painted - Steel gray',0.592156862745098,
0.631372549019608,0.67843137254902);
#34486=COLOUR_RGB('CAD Library Painted - Engineering blue',0.12156862745098,
0.356862745098039,0.6);
#34487=COLOUR_RGB('CAD Library Painted - Off white',0.909803921568627,0.901960784313726,
0.858823529411765);
#34488=COLOUR_RGB('CAD Library Painted - Graphite',0.0980392156862745,0.109803921568627,
0.125490196078431);
#34489=COLOUR_RGB('CAD Library Painted - Light blue',0.286274509803922,
0.552941176470588,0.780392156862745);
#34490=COLOUR_RGB('Dark Blue',0.08,0.2,0.34);
#34491=FILL_AREA_STYLE_COLOUR('',#34490);
#34492=FILL_AREA_STYLE('',(#34491));
#34493=SURFACE_STYLE_FILL_AREA(#34492);
#34494=SURFACE_SIDE_STYLE('',(#34493));
#34495=SURFACE_STYLE_USAGE(.BOTH.,#34494);
#34496=PRESENTATION_STYLE_ASSIGNMENT((#34495));
#34497=COLOUR_RGB('Light Blue',0.38,0.62,0.78);
#34498=FILL_AREA_STYLE_COLOUR('',#34497);
#34499=FILL_AREA_STYLE('',(#34498));
#34500=SURFACE_STYLE_FILL_AREA(#34499);
#34501=SURFACE_SIDE_STYLE('',(#34500));
#34502=SURFACE_STYLE_USAGE(.BOTH.,#34501);
#34503=PRESENTATION_STYLE_ASSIGNMENT((#34502));
#34504=COLOUR_RGB('Sky Blue',0.24,0.69,0.87);
#34505=FILL_AREA_STYLE_COLOUR('',#34504);
#34506=FILL_AREA_STYLE('',(#34505));
#34507=SURFACE_STYLE_FILL_AREA(#34506);
#34508=SURFACE_SIDE_STYLE('',(#34507));
#34509=SURFACE_STYLE_USAGE(.BOTH.,#34508);
#34510=PRESENTATION_STYLE_ASSIGNMENT((#34509));
#34511=COLOUR_RGB('Grey',0.48,0.52,0.57);
#34512=FILL_AREA_STYLE_COLOUR('',#34511);
#34513=FILL_AREA_STYLE('',(#34512));
#34514=SURFACE_STYLE_FILL_AREA(#34513);
#34515=SURFACE_SIDE_STYLE('',(#34514));
#34516=SURFACE_STYLE_USAGE(.BOTH.,#34515);
#34517=PRESENTATION_STYLE_ASSIGNMENT((#34516));
#34518=COLOUR_RGB('Black',0.12,0.14,0.17);
#34519=FILL_AREA_STYLE_COLOUR('',#34518);
#34520=FILL_AREA_STYLE('',(#34519));
#34521=SURFACE_STYLE_FILL_AREA(#34520);
#34522=SURFACE_SIDE_STYLE('',(#34521));
#34523=SURFACE_STYLE_USAGE(.BOTH.,#34522);
#34524=PRESENTATION_STYLE_ASSIGNMENT((#34523));
#34525=COLOUR_RGB('Off White',0.89,0.88,0.83);
#34526=FILL_AREA_STYLE_COLOUR('',#34525);
#34527=FILL_AREA_STYLE('',(#34526));
#34528=SURFACE_STYLE_FILL_AREA(#34527);
#34529=SURFACE_SIDE_STYLE('',(#34528));
#34530=SURFACE_STYLE_USAGE(.BOTH.,#34529);
#34531=PRESENTATION_STYLE_ASSIGNMENT((#34530));
ENDSEC;
END-ISO-10303-21;
